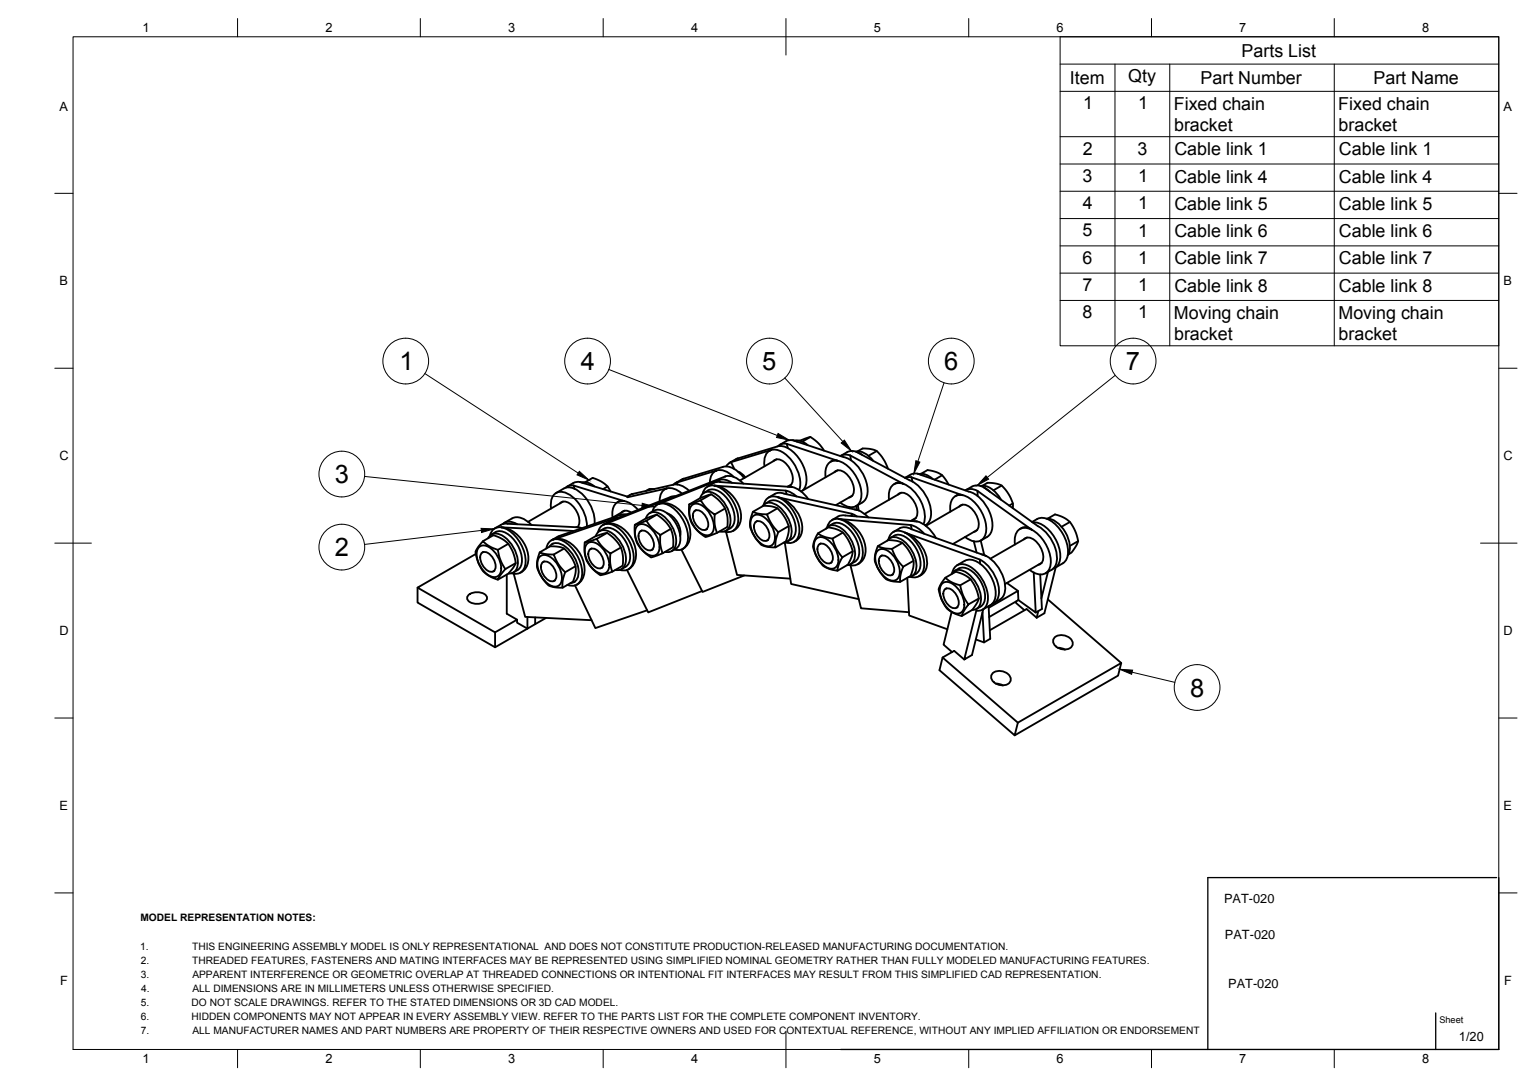
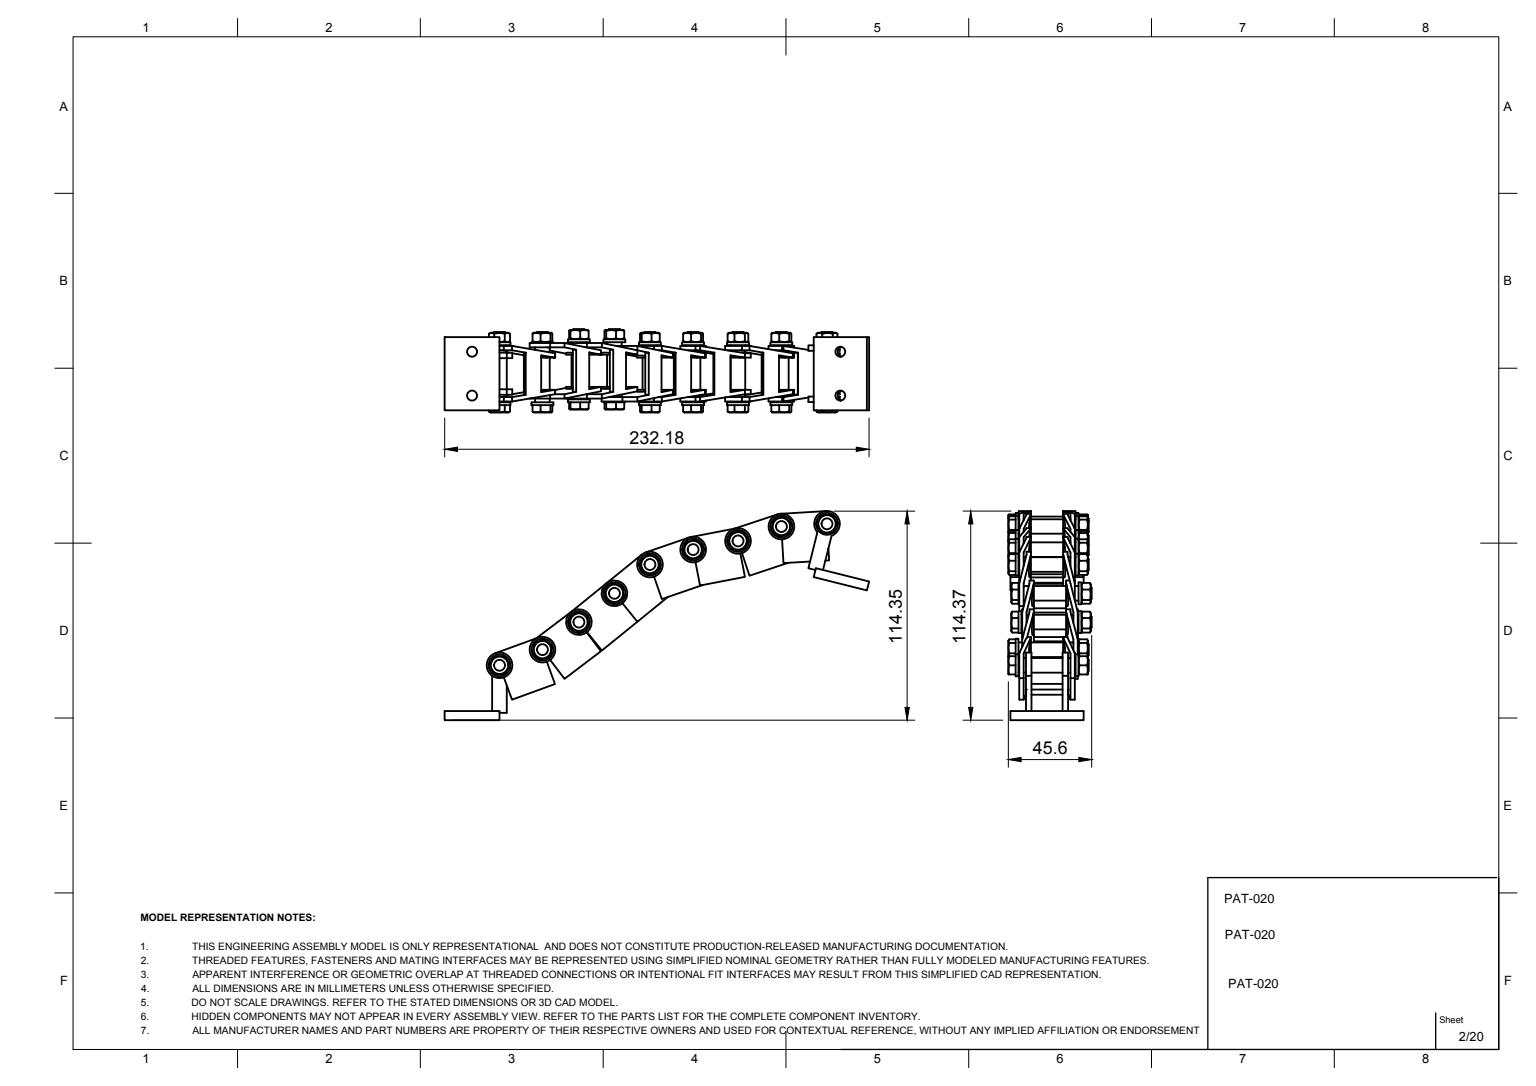
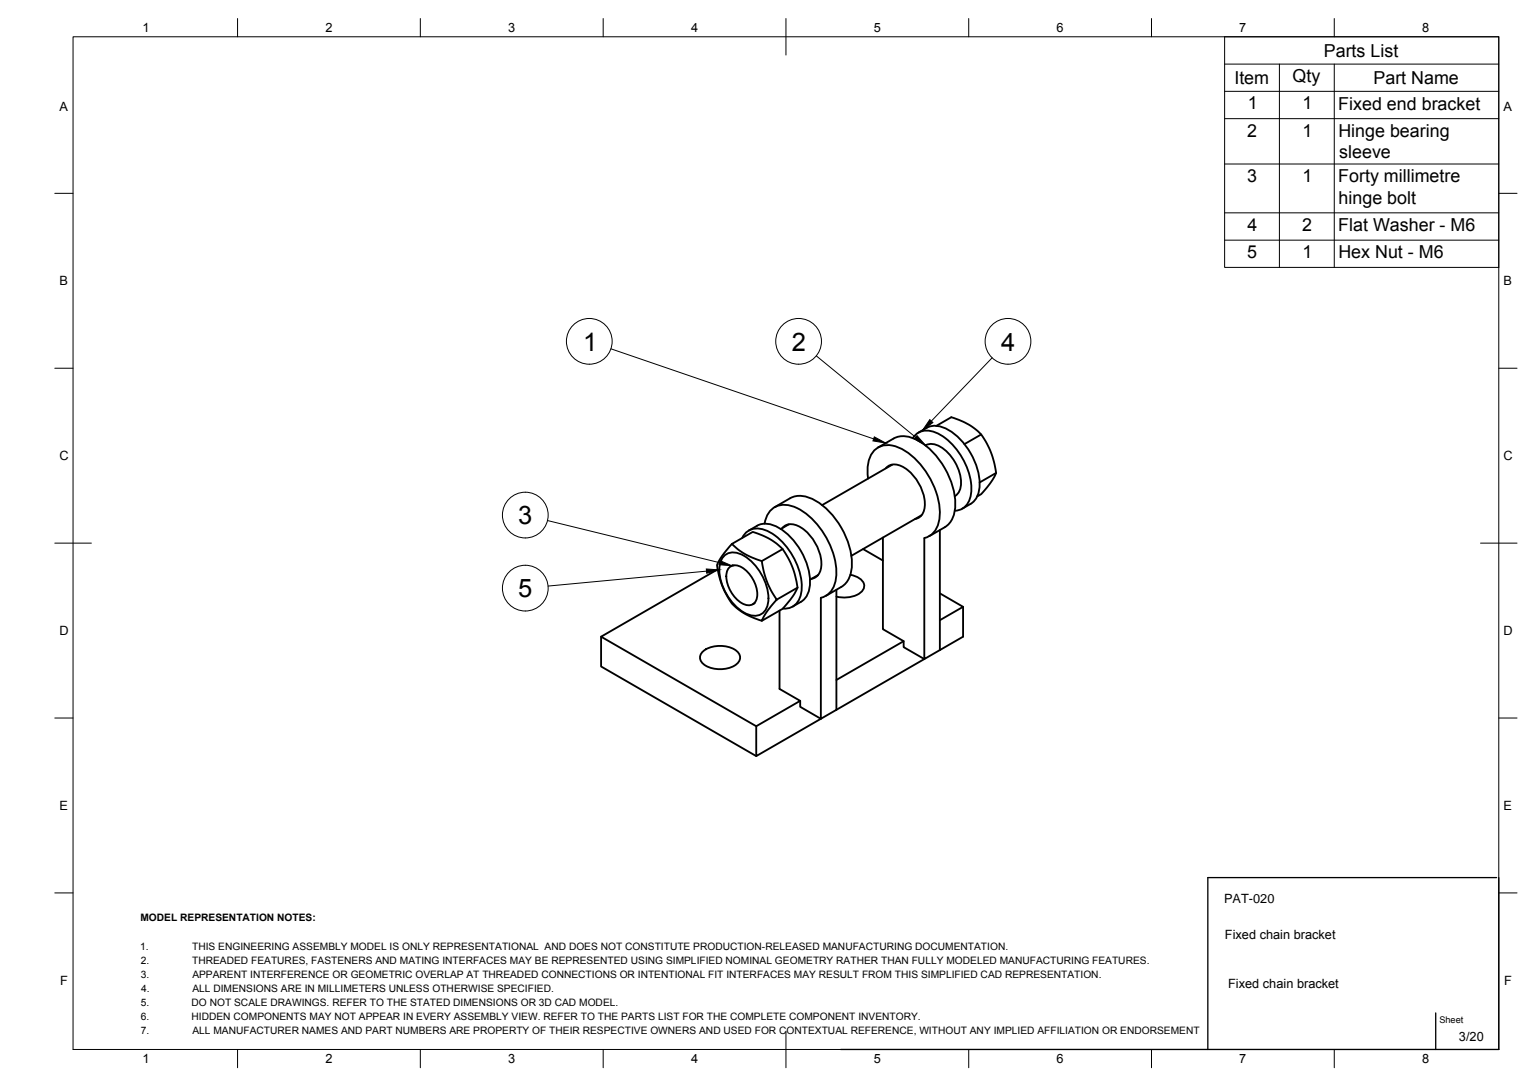
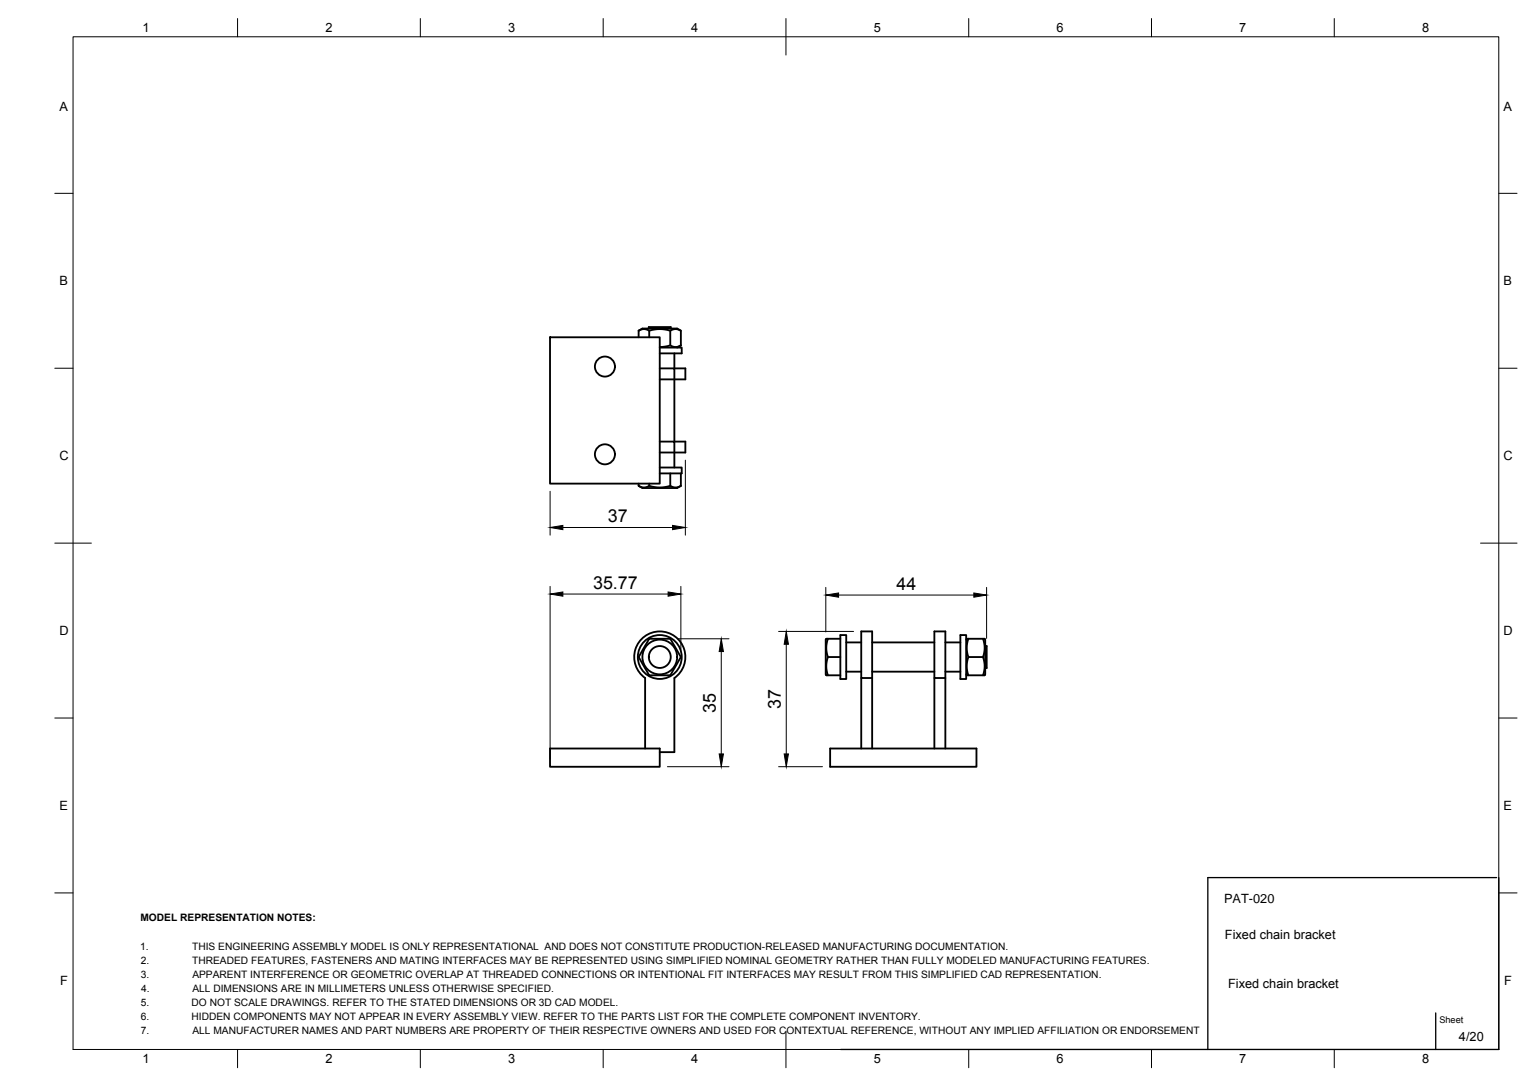
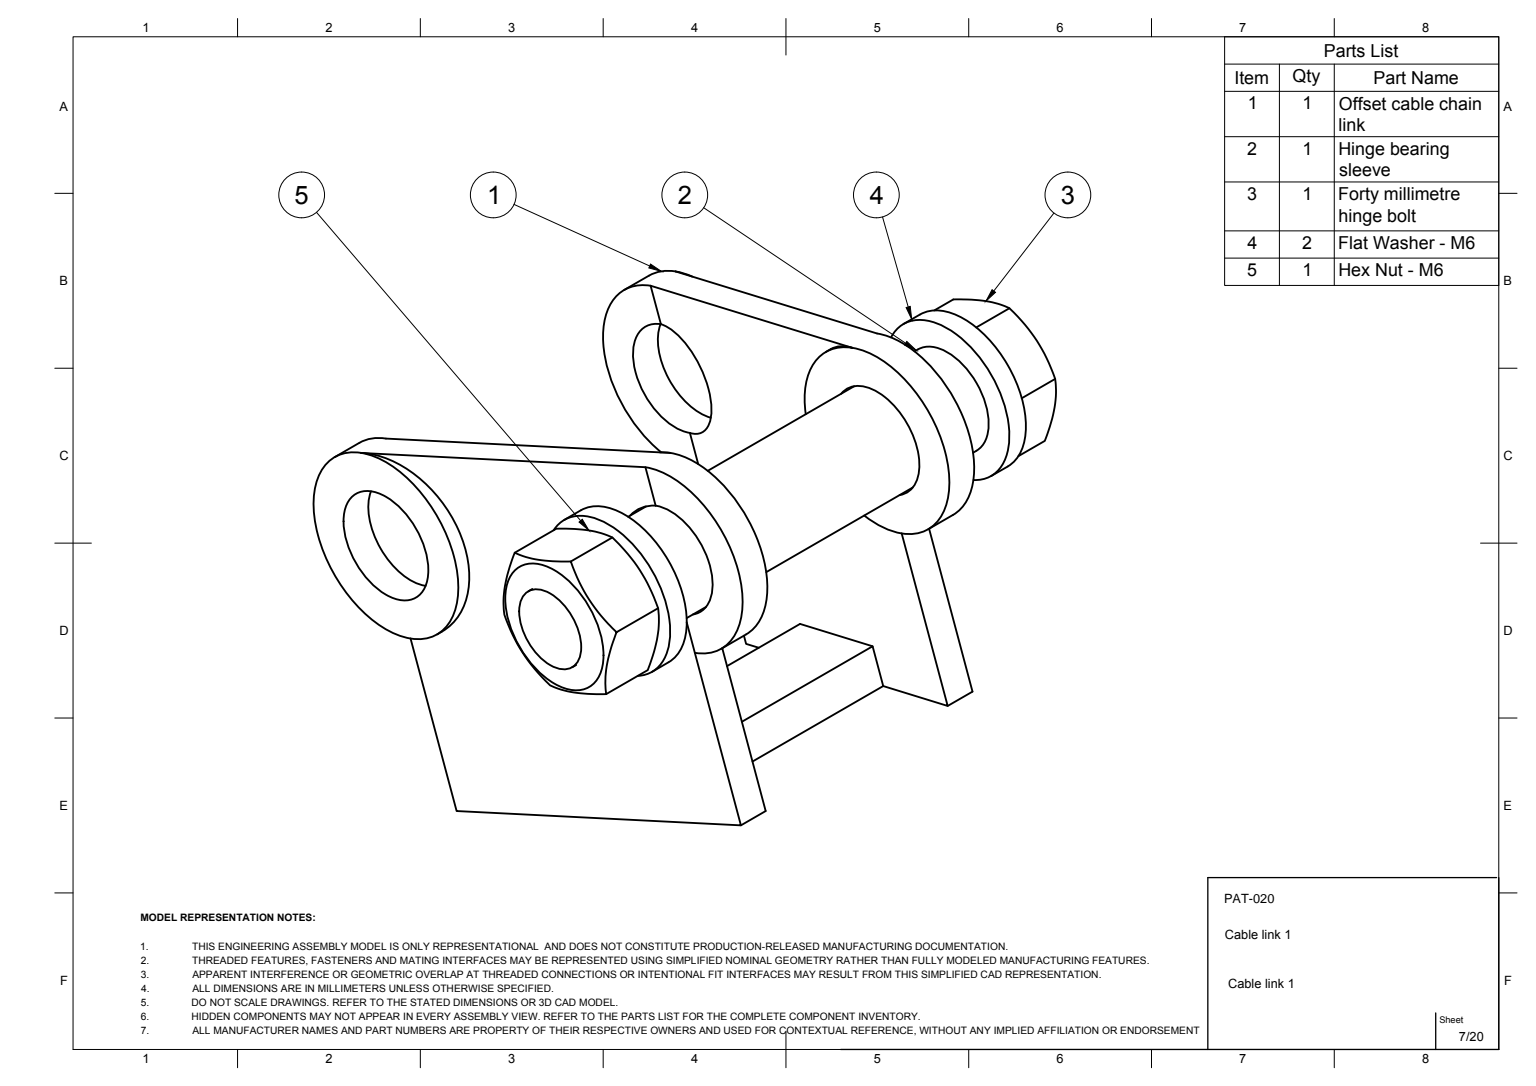
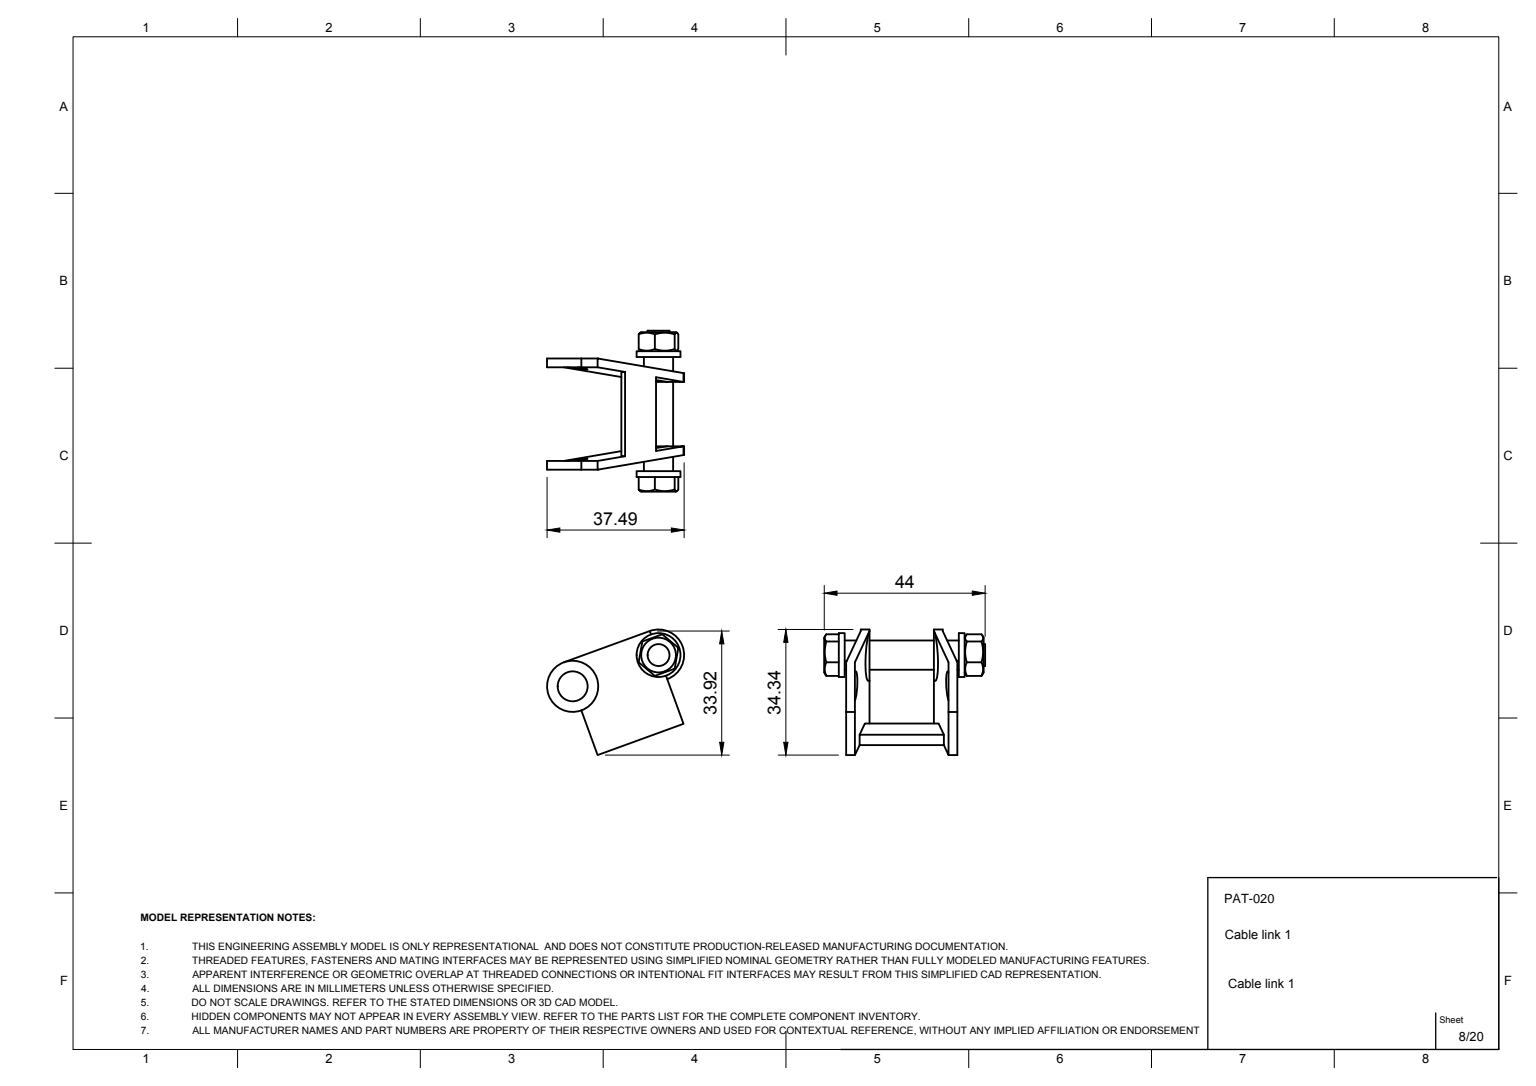
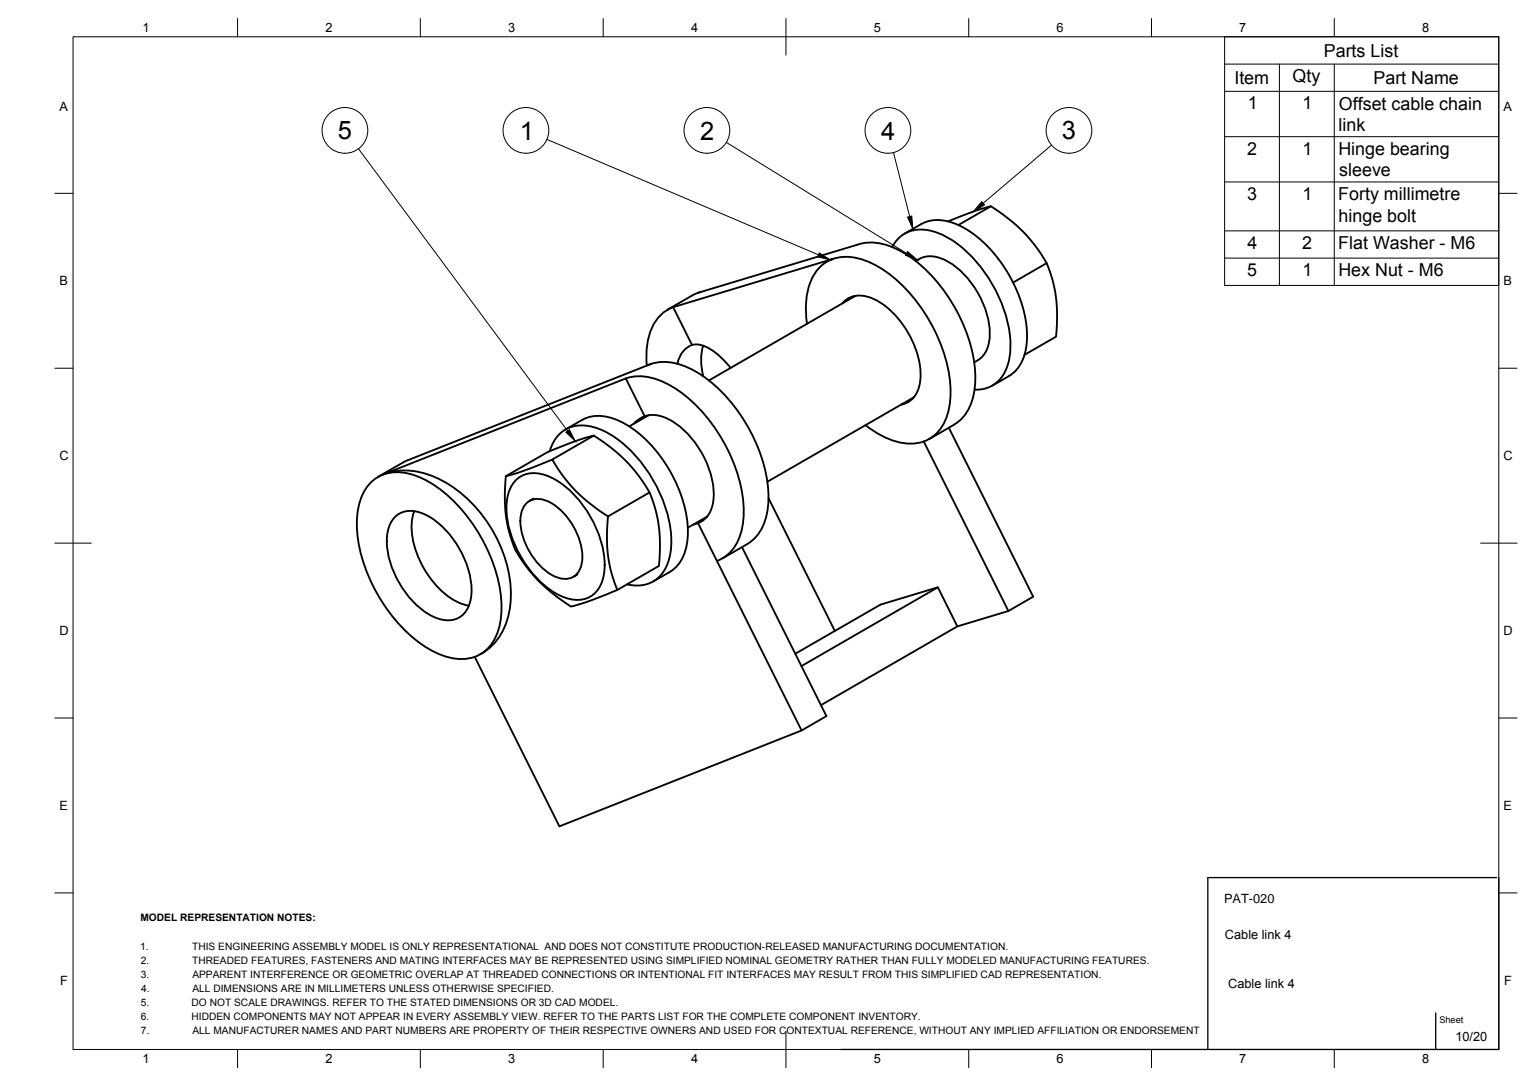
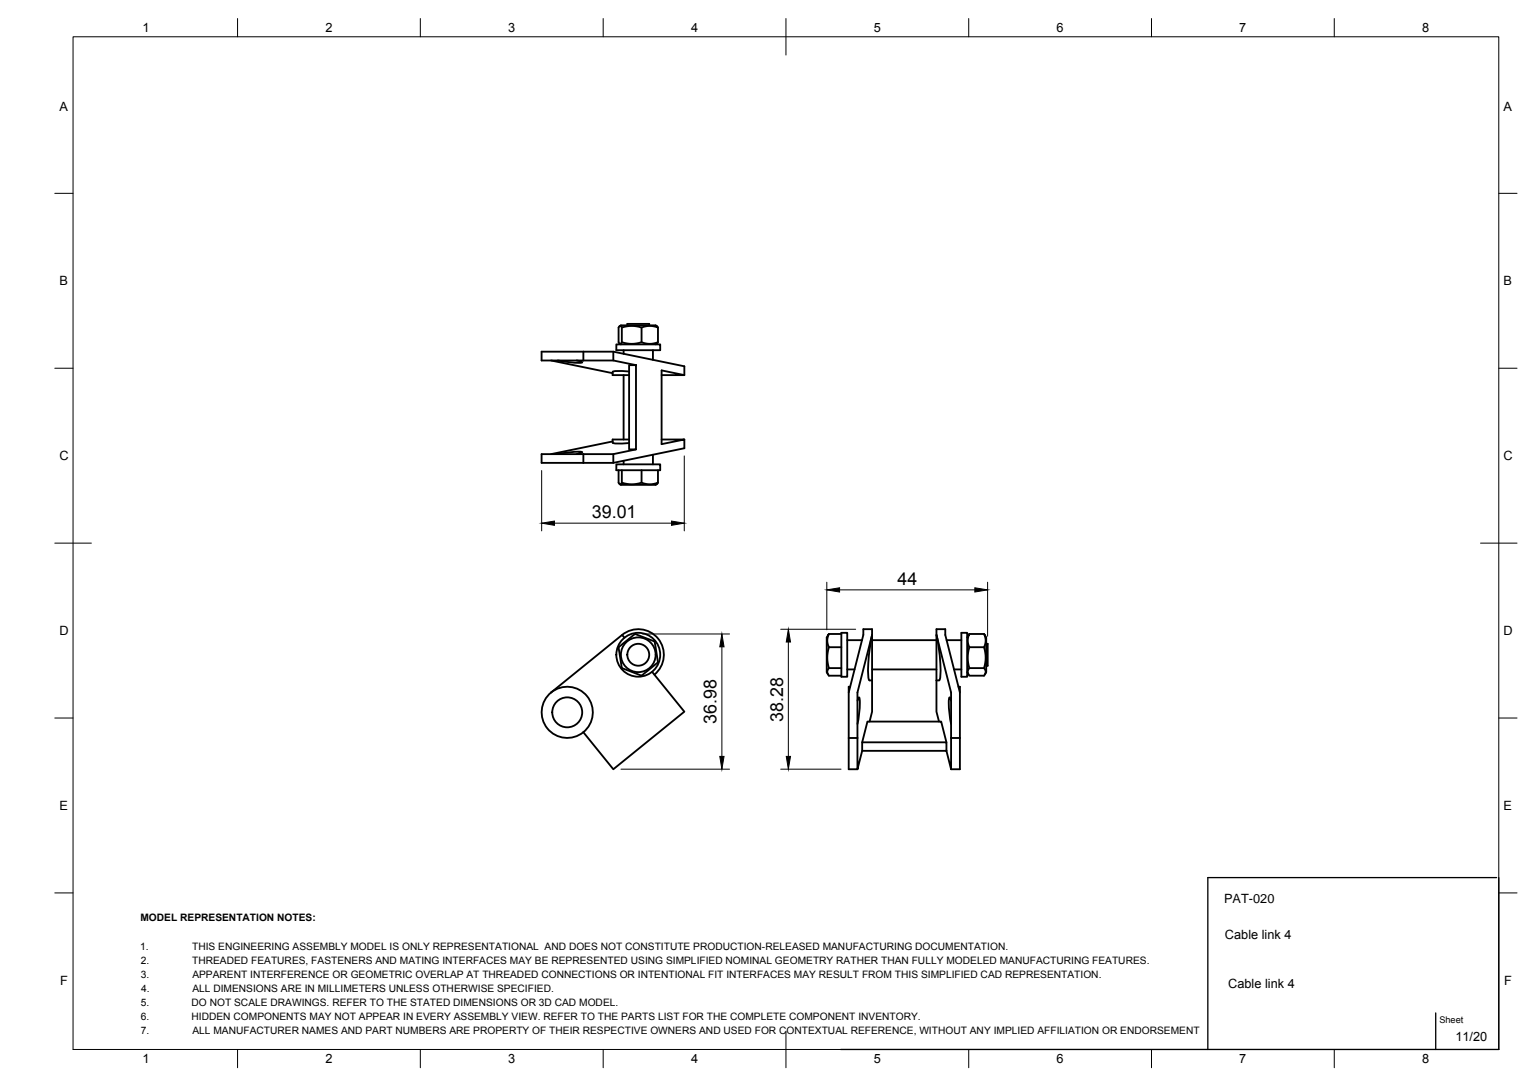
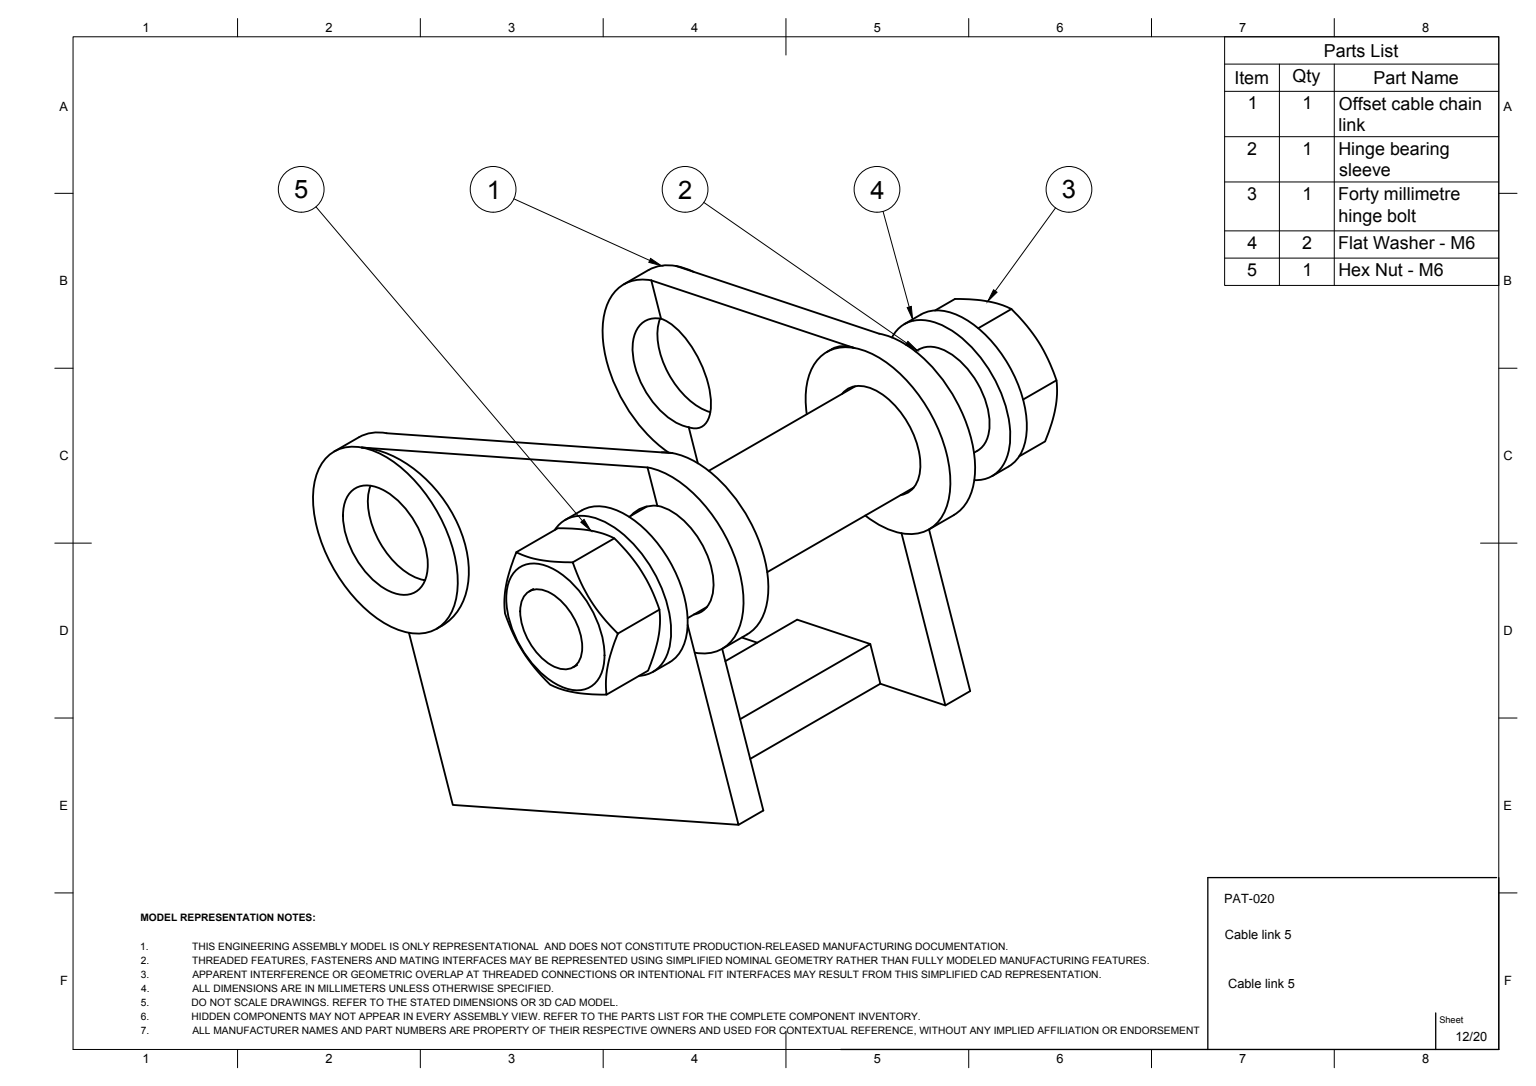
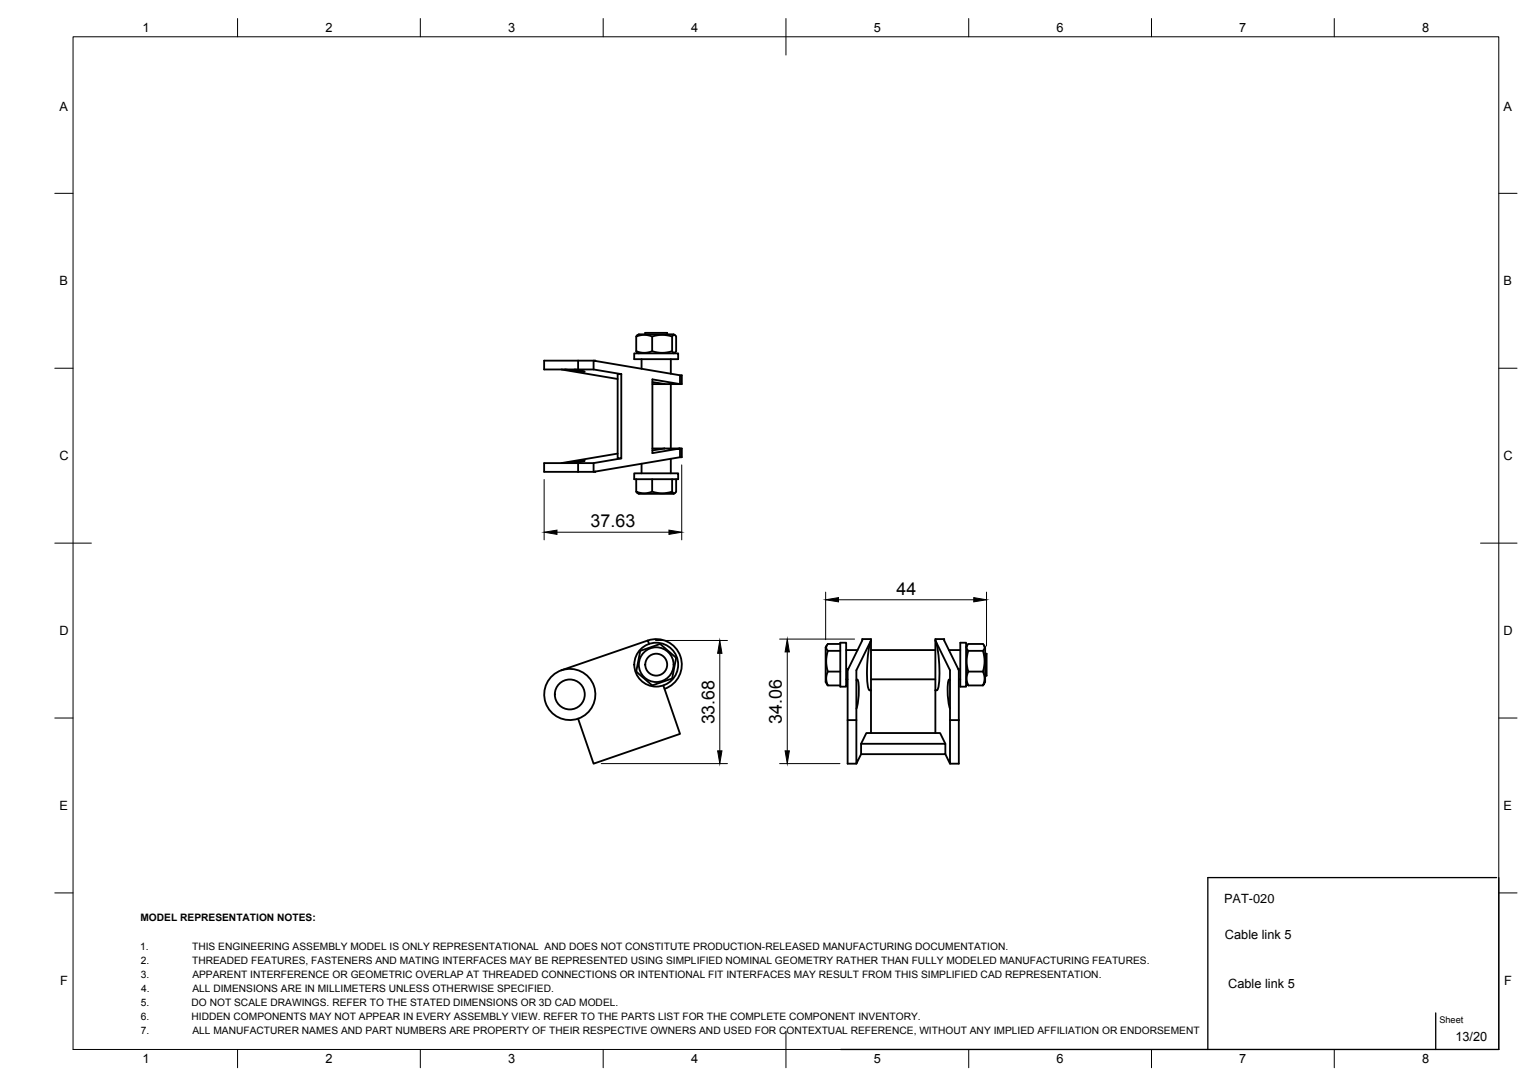
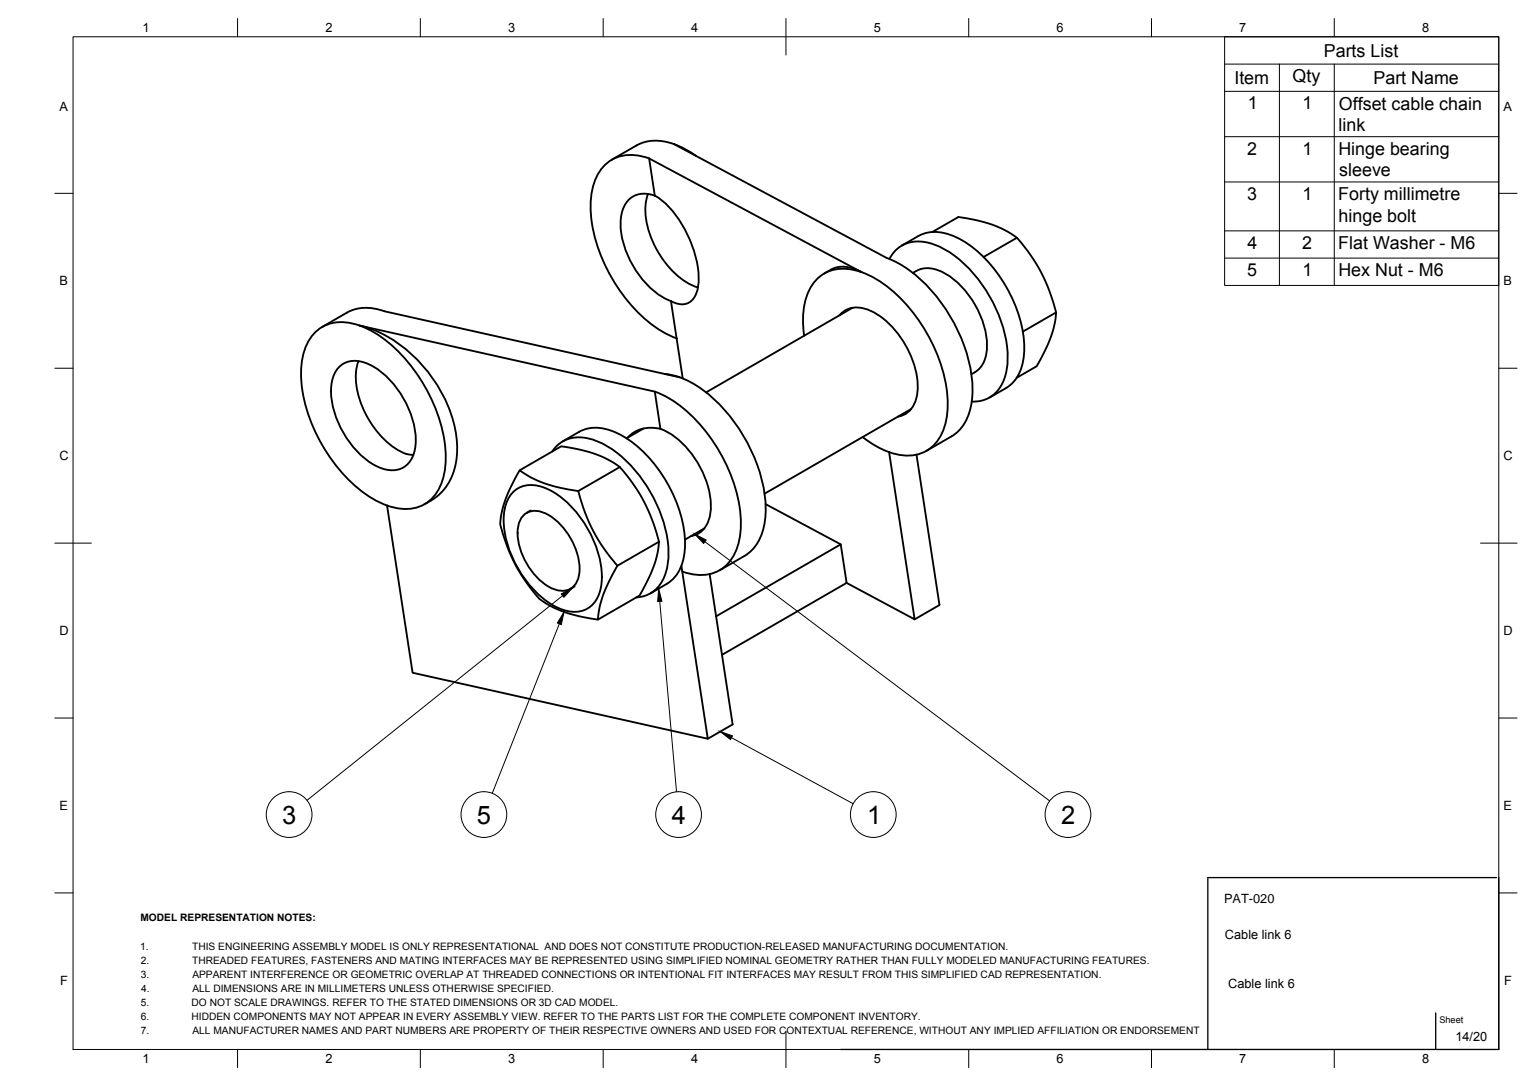
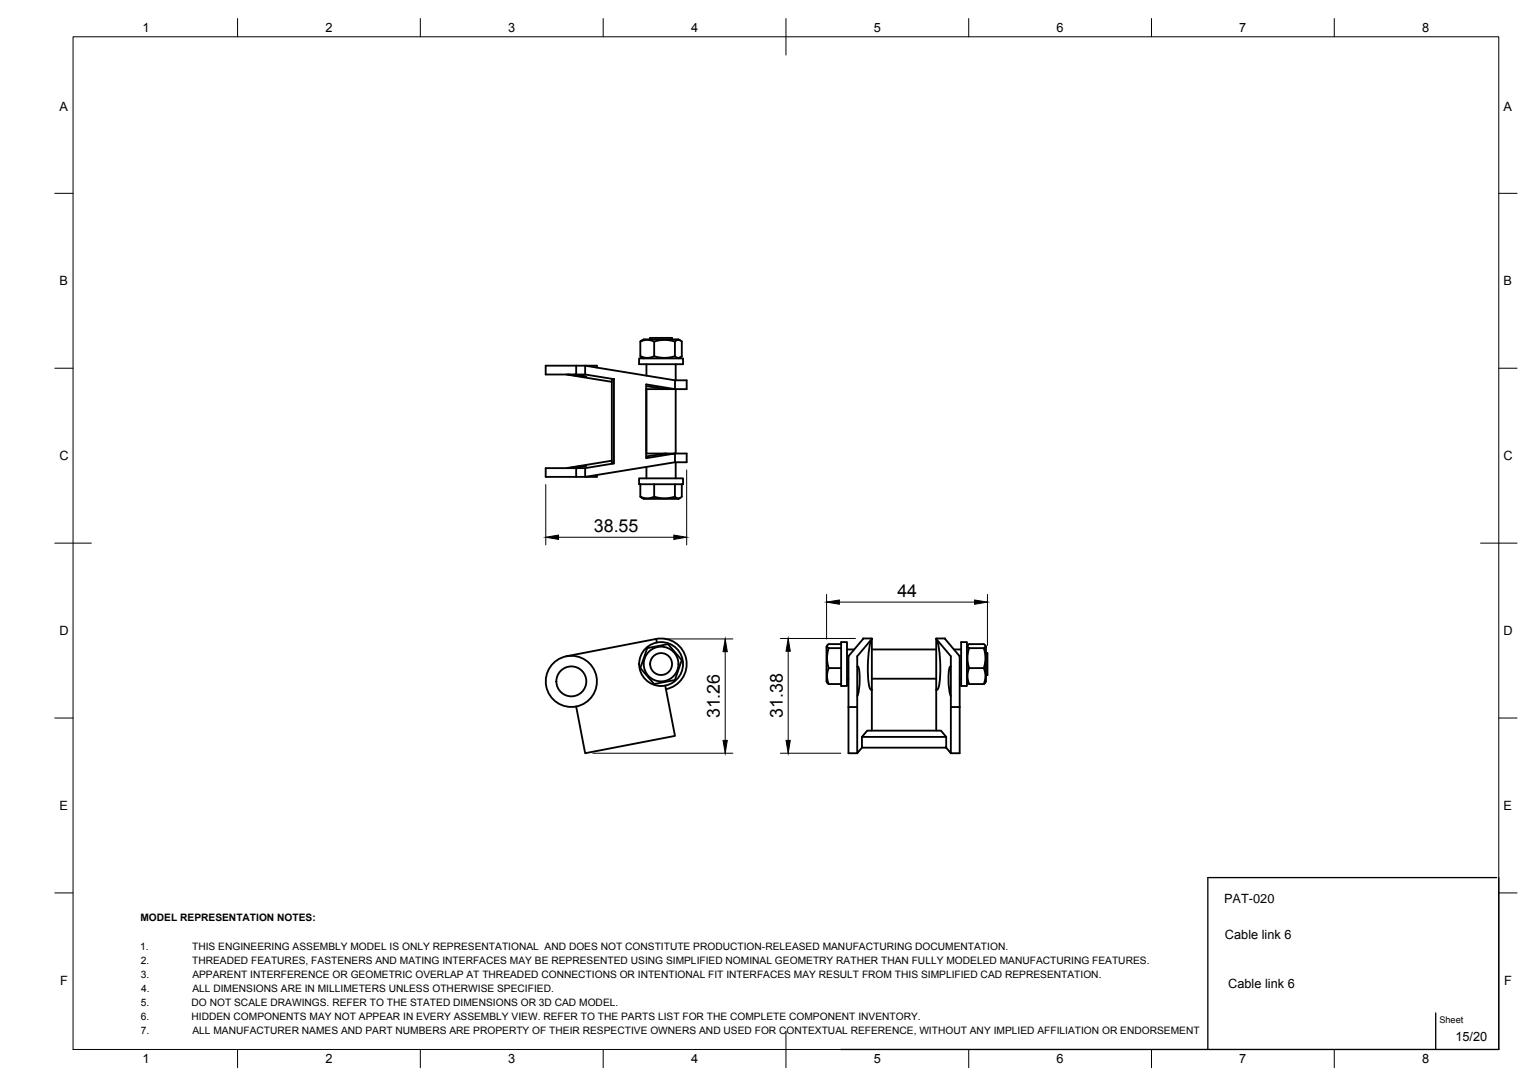
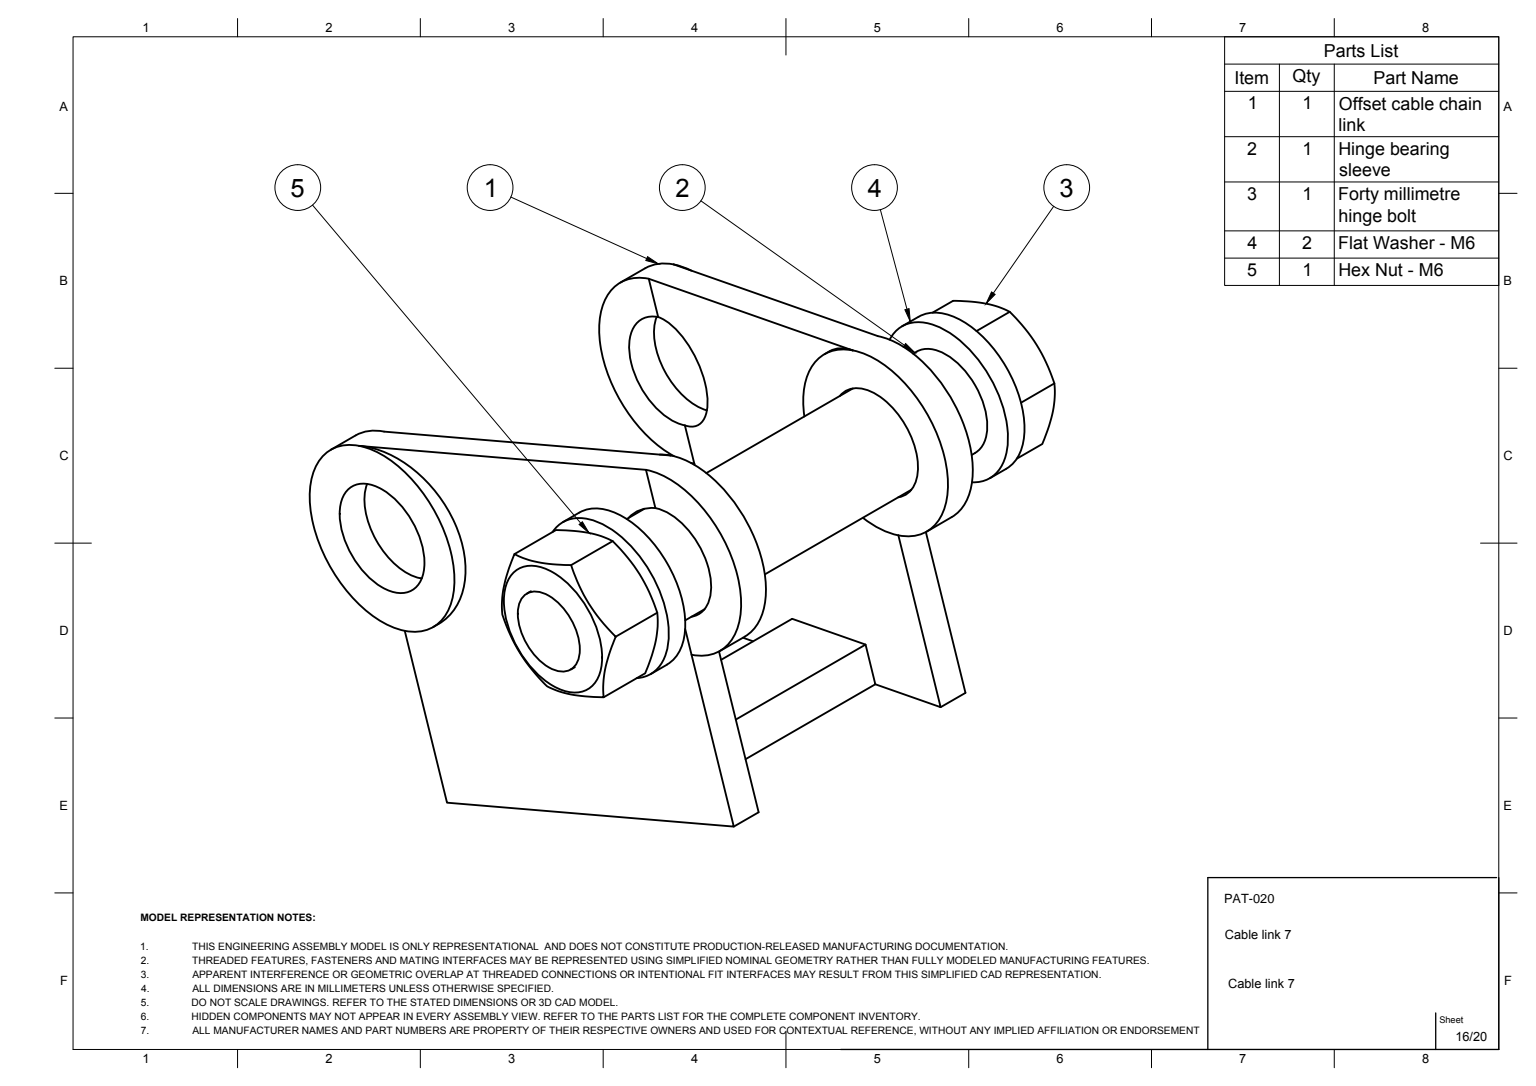
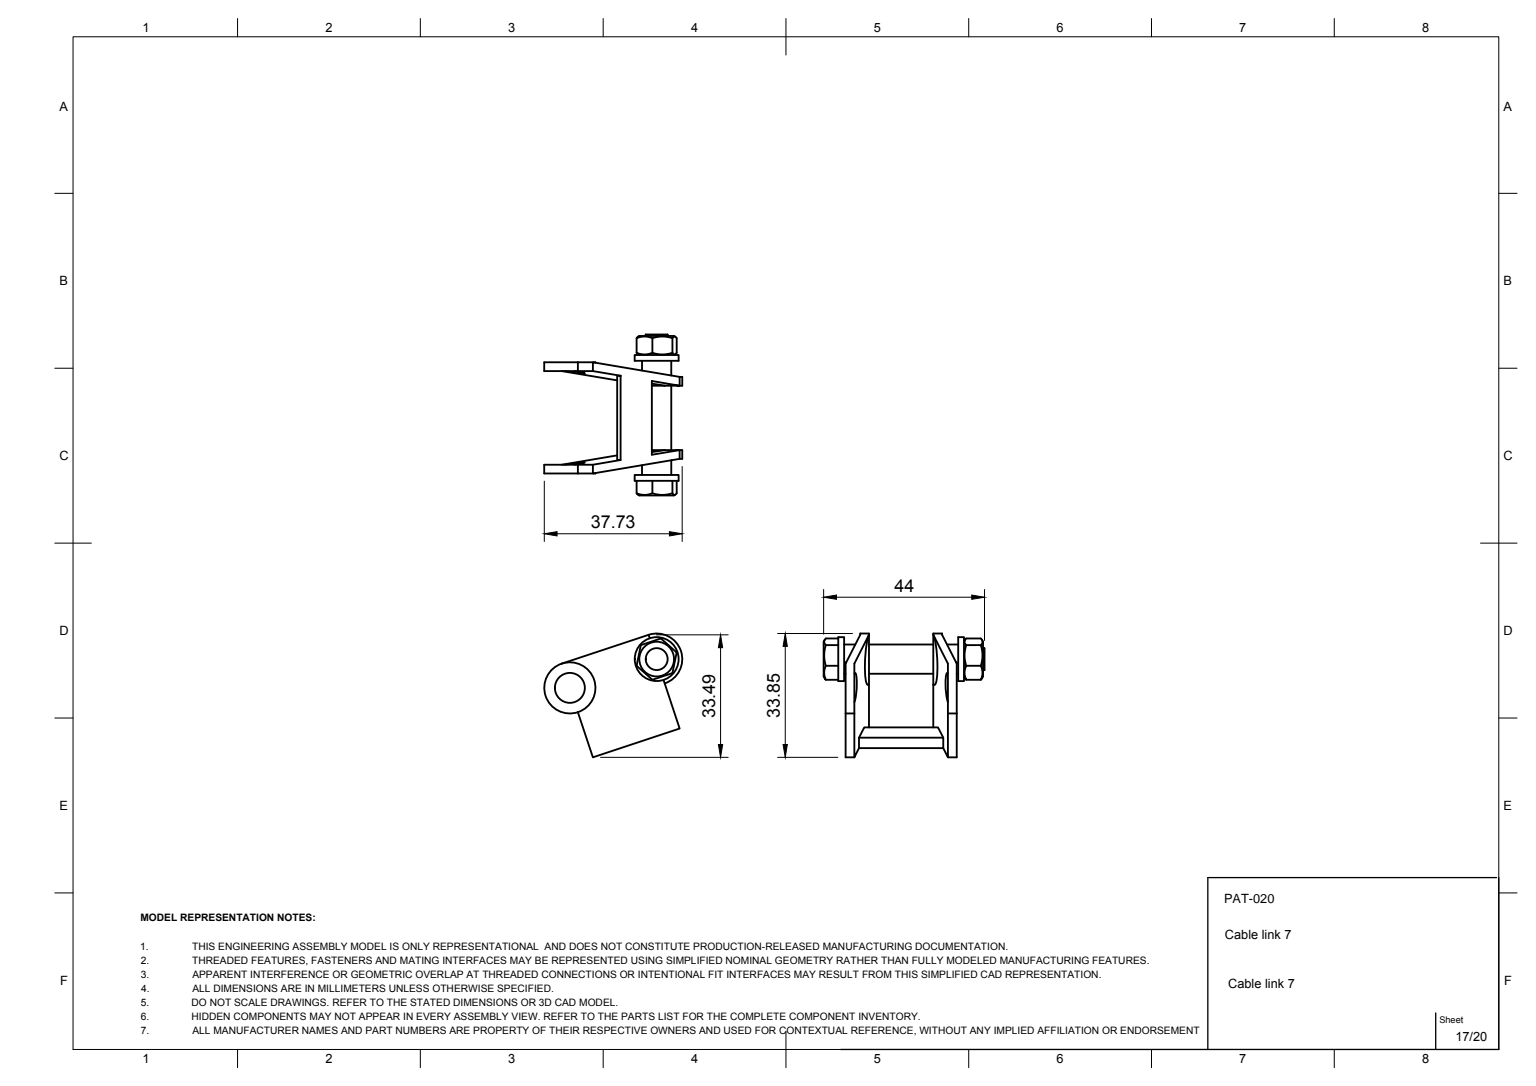
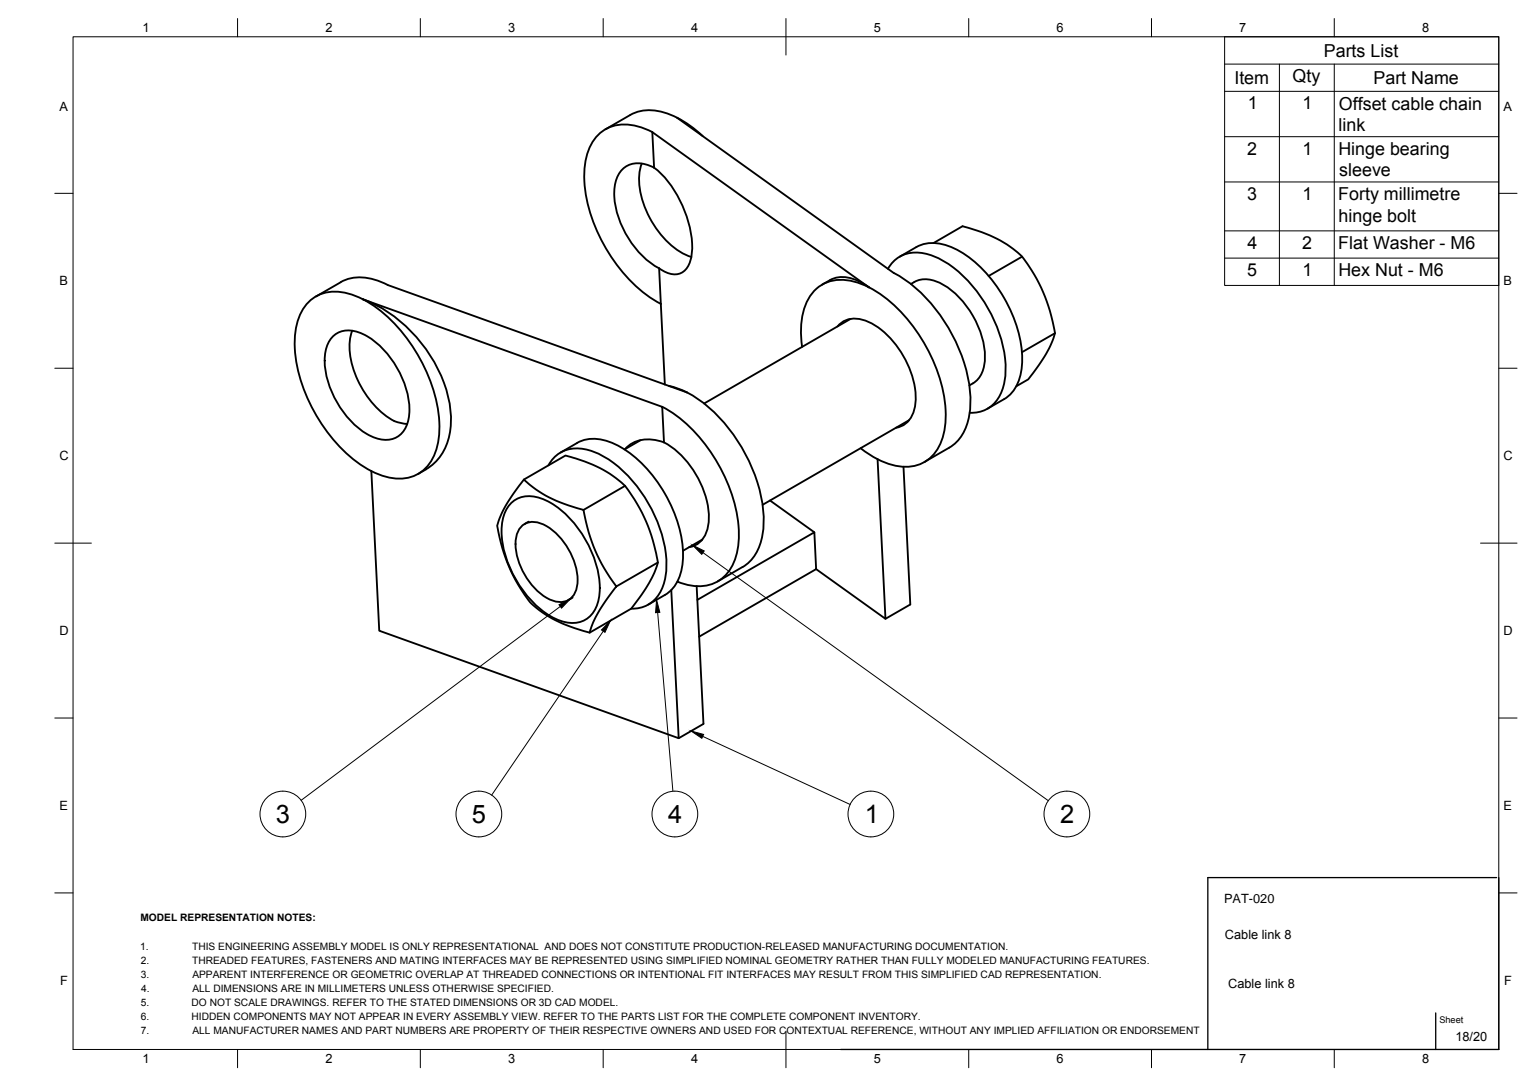
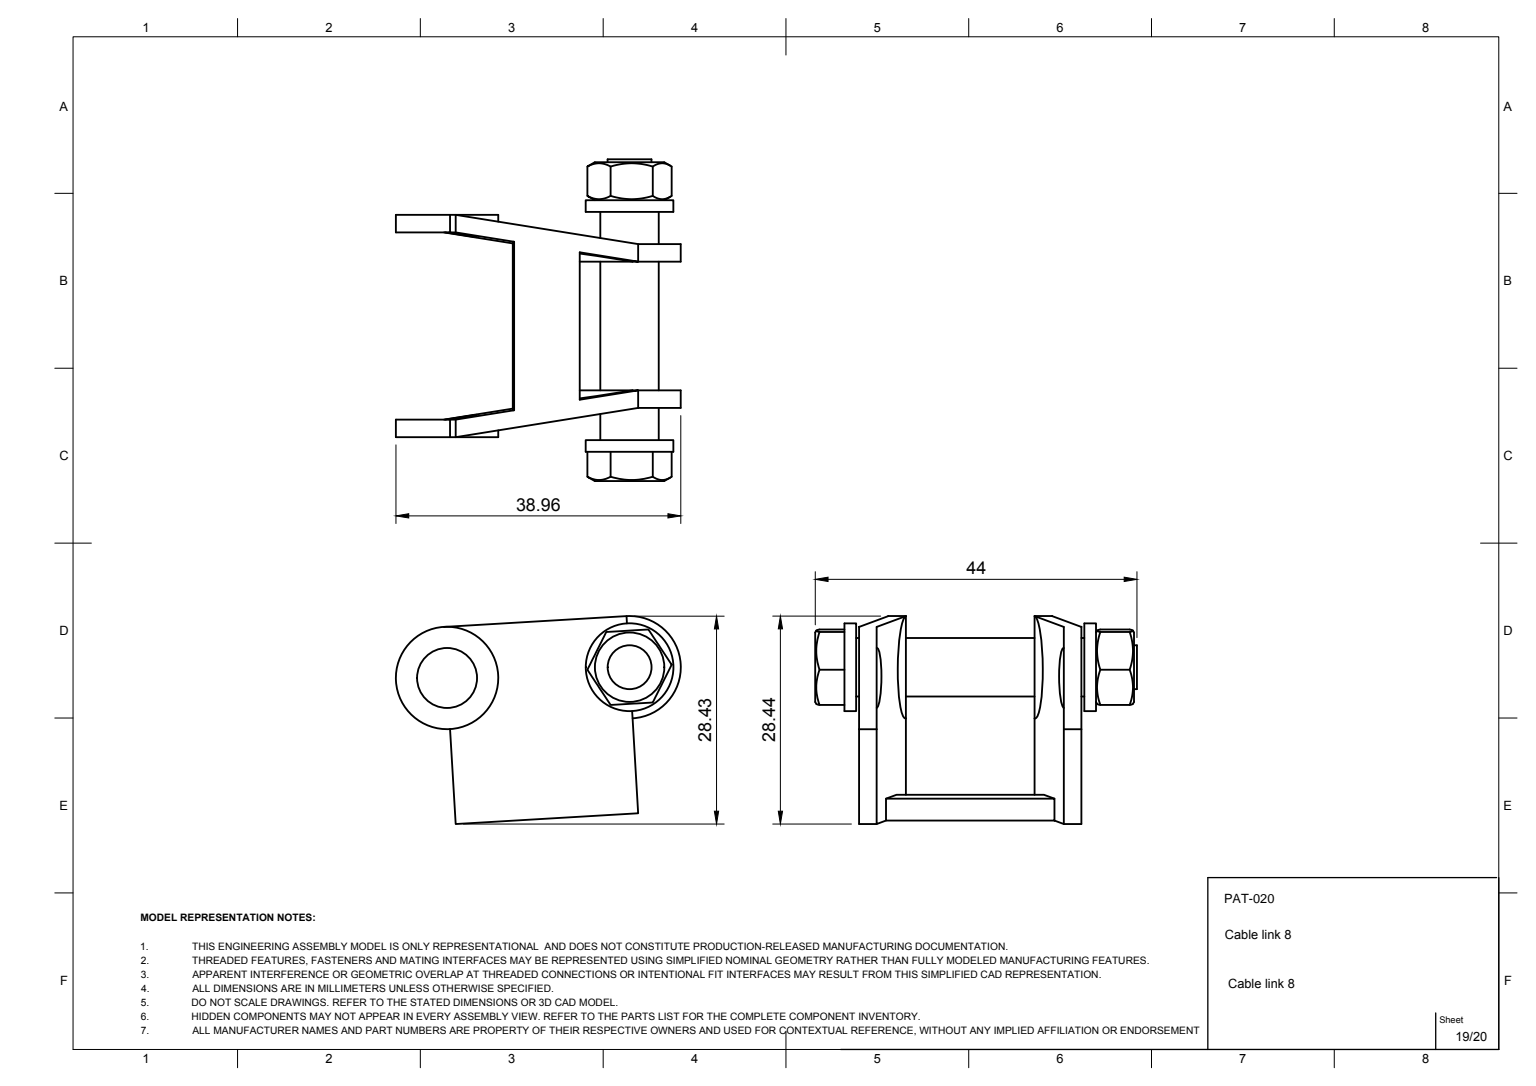
ISO-10303-21;
HEADER;
/* Generated by software containing ST-Developer
 * from STEP Tools, Inc. (www.steptools.com) 
 */

FILE_DESCRIPTION(
/* description */ ('Cable chain and bracket set'),
/* implementation_level */ '2;1');

FILE_NAME(
/* name */ 'PAT-020',
/* time_stamp */ '2026-10-29T17:19:47-07:00',
/* author */ (''),
/* organization */ (''),
/* preprocessor_version */ 'ST-DEVELOPER v20.2',
/* originating_system */ 'Autodesk Translation Framework v15.17.0.0',
/* authorisation */ '');

FILE_SCHEMA (('AUTOMOTIVE_DESIGN { 1 0 10303 214 3 1 1 }'));
ENDSEC;

DATA;
#10=MECHANICAL_DESIGN_GEOMETRIC_PRESENTATION_REPRESENTATION('',(#337,#338,
#339,#340,#341,#342,#343,#344,#345,#346,#347,#348,#349),#5929);
#11=ITEM_DEFINED_TRANSFORMATION($,$,#3460,#3591);
#12=ITEM_DEFINED_TRANSFORMATION($,$,#3527,#3592);
#13=ITEM_DEFINED_TRANSFORMATION($,$,#3536,#3593);
#14=ITEM_DEFINED_TRANSFORMATION($,$,#3557,#3594);
#15=ITEM_DEFINED_TRANSFORMATION($,$,#3566,#3595);
#16=ITEM_DEFINED_TRANSFORMATION($,$,#3575,#3596);
#17=ITEM_DEFINED_TRANSFORMATION($,$,#3603,#3638);
#18=ITEM_DEFINED_TRANSFORMATION($,$,#3424,#3762);
#19=ITEM_DEFINED_TRANSFORMATION($,$,#3707,#3763);
#20=ITEM_DEFINED_TRANSFORMATION($,$,#3716,#3764);
#21=ITEM_DEFINED_TRANSFORMATION($,$,#3737,#3765);
#22=ITEM_DEFINED_TRANSFORMATION($,$,#3737,#3766);
#23=ITEM_DEFINED_TRANSFORMATION($,$,#3746,#3767);
#24=ITEM_DEFINED_TRANSFORMATION($,$,#3640,#3768);
#25=ITEM_DEFINED_TRANSFORMATION($,$,#3707,#3769);
#26=ITEM_DEFINED_TRANSFORMATION($,$,#3716,#3770);
#27=ITEM_DEFINED_TRANSFORMATION($,$,#3737,#3771);
#28=ITEM_DEFINED_TRANSFORMATION($,$,#3737,#3772);
#29=ITEM_DEFINED_TRANSFORMATION($,$,#3746,#3773);
#30=ITEM_DEFINED_TRANSFORMATION($,$,#3640,#3774);
#31=ITEM_DEFINED_TRANSFORMATION($,$,#3707,#3775);
#32=ITEM_DEFINED_TRANSFORMATION($,$,#3716,#3776);
#33=ITEM_DEFINED_TRANSFORMATION($,$,#3737,#3777);
#34=ITEM_DEFINED_TRANSFORMATION($,$,#3737,#3778);
#35=ITEM_DEFINED_TRANSFORMATION($,$,#3746,#3779);
#36=ITEM_DEFINED_TRANSFORMATION($,$,#3640,#3780);
#37=ITEM_DEFINED_TRANSFORMATION($,$,#3707,#3781);
#38=ITEM_DEFINED_TRANSFORMATION($,$,#3716,#3782);
#39=ITEM_DEFINED_TRANSFORMATION($,$,#3737,#3783);
#40=ITEM_DEFINED_TRANSFORMATION($,$,#3737,#3784);
#41=ITEM_DEFINED_TRANSFORMATION($,$,#3746,#3785);
#42=ITEM_DEFINED_TRANSFORMATION($,$,#3640,#3786);
#43=ITEM_DEFINED_TRANSFORMATION($,$,#3707,#3787);
#44=ITEM_DEFINED_TRANSFORMATION($,$,#3716,#3788);
#45=ITEM_DEFINED_TRANSFORMATION($,$,#3737,#3789);
#46=ITEM_DEFINED_TRANSFORMATION($,$,#3737,#3790);
#47=ITEM_DEFINED_TRANSFORMATION($,$,#3746,#3791);
#48=ITEM_DEFINED_TRANSFORMATION($,$,#3640,#3792);
#49=ITEM_DEFINED_TRANSFORMATION($,$,#3707,#3793);
#50=ITEM_DEFINED_TRANSFORMATION($,$,#3716,#3794);
#51=ITEM_DEFINED_TRANSFORMATION($,$,#3737,#3795);
#52=ITEM_DEFINED_TRANSFORMATION($,$,#3737,#3796);
#53=ITEM_DEFINED_TRANSFORMATION($,$,#3746,#3797);
#54=ITEM_DEFINED_TRANSFORMATION($,$,#3640,#3798);
#55=ITEM_DEFINED_TRANSFORMATION($,$,#3707,#3799);
#56=ITEM_DEFINED_TRANSFORMATION($,$,#3716,#3800);
#57=ITEM_DEFINED_TRANSFORMATION($,$,#3737,#3801);
#58=ITEM_DEFINED_TRANSFORMATION($,$,#3737,#3802);
#59=ITEM_DEFINED_TRANSFORMATION($,$,#3746,#3803);
#60=ITEM_DEFINED_TRANSFORMATION($,$,#3423,#3804);
#61=ITEM_DEFINED_TRANSFORMATION($,$,#3459,#3805);
#62=ITEM_DEFINED_TRANSFORMATION($,$,#3597,#3806);
#63=ITEM_DEFINED_TRANSFORMATION($,$,#3598,#3807);
#64=ITEM_DEFINED_TRANSFORMATION($,$,#3599,#3808);
#65=ITEM_DEFINED_TRANSFORMATION($,$,#3600,#3809);
#66=ITEM_DEFINED_TRANSFORMATION($,$,#3601,#3810);
#67=ITEM_DEFINED_TRANSFORMATION($,$,#3602,#3811);
#68=ITEM_DEFINED_TRANSFORMATION($,$,#3639,#3812);
#69=ITEM_DEFINED_TRANSFORMATION($,$,#3639,#3813);
#70=(
REPRESENTATION_RELATIONSHIP($,$,#6043,#6042)
REPRESENTATION_RELATIONSHIP_WITH_TRANSFORMATION(#11)
SHAPE_REPRESENTATION_RELATIONSHIP()
);
#71=(
REPRESENTATION_RELATIONSHIP($,$,#6044,#6042)
REPRESENTATION_RELATIONSHIP_WITH_TRANSFORMATION(#12)
SHAPE_REPRESENTATION_RELATIONSHIP()
);
#72=(
REPRESENTATION_RELATIONSHIP($,$,#6045,#6042)
REPRESENTATION_RELATIONSHIP_WITH_TRANSFORMATION(#13)
SHAPE_REPRESENTATION_RELATIONSHIP()
);
#73=(
REPRESENTATION_RELATIONSHIP($,$,#6046,#6042)
REPRESENTATION_RELATIONSHIP_WITH_TRANSFORMATION(#14)
SHAPE_REPRESENTATION_RELATIONSHIP()
);
#74=(
REPRESENTATION_RELATIONSHIP($,$,#6047,#6042)
REPRESENTATION_RELATIONSHIP_WITH_TRANSFORMATION(#15)
SHAPE_REPRESENTATION_RELATIONSHIP()
);
#75=(
REPRESENTATION_RELATIONSHIP($,$,#6048,#6042)
REPRESENTATION_RELATIONSHIP_WITH_TRANSFORMATION(#16)
SHAPE_REPRESENTATION_RELATIONSHIP()
);
#76=(
REPRESENTATION_RELATIONSHIP($,$,#6055,#6054)
REPRESENTATION_RELATIONSHIP_WITH_TRANSFORMATION(#17)
SHAPE_REPRESENTATION_RELATIONSHIP()
);
#77=(
REPRESENTATION_RELATIONSHIP($,$,#6041,#6040)
REPRESENTATION_RELATIONSHIP_WITH_TRANSFORMATION(#18)
SHAPE_REPRESENTATION_RELATIONSHIP()
);
#78=(
REPRESENTATION_RELATIONSHIP($,$,#6058,#6040)
REPRESENTATION_RELATIONSHIP_WITH_TRANSFORMATION(#19)
SHAPE_REPRESENTATION_RELATIONSHIP()
);
#79=(
REPRESENTATION_RELATIONSHIP($,$,#6059,#6040)
REPRESENTATION_RELATIONSHIP_WITH_TRANSFORMATION(#20)
SHAPE_REPRESENTATION_RELATIONSHIP()
);
#80=(
REPRESENTATION_RELATIONSHIP($,$,#6060,#6040)
REPRESENTATION_RELATIONSHIP_WITH_TRANSFORMATION(#21)
SHAPE_REPRESENTATION_RELATIONSHIP()
);
#81=(
REPRESENTATION_RELATIONSHIP($,$,#6060,#6040)
REPRESENTATION_RELATIONSHIP_WITH_TRANSFORMATION(#22)
SHAPE_REPRESENTATION_RELATIONSHIP()
);
#82=(
REPRESENTATION_RELATIONSHIP($,$,#6061,#6040)
REPRESENTATION_RELATIONSHIP_WITH_TRANSFORMATION(#23)
SHAPE_REPRESENTATION_RELATIONSHIP()
);
#83=(
REPRESENTATION_RELATIONSHIP($,$,#6057,#6049)
REPRESENTATION_RELATIONSHIP_WITH_TRANSFORMATION(#24)
SHAPE_REPRESENTATION_RELATIONSHIP()
);
#84=(
REPRESENTATION_RELATIONSHIP($,$,#6058,#6049)
REPRESENTATION_RELATIONSHIP_WITH_TRANSFORMATION(#25)
SHAPE_REPRESENTATION_RELATIONSHIP()
);
#85=(
REPRESENTATION_RELATIONSHIP($,$,#6059,#6049)
REPRESENTATION_RELATIONSHIP_WITH_TRANSFORMATION(#26)
SHAPE_REPRESENTATION_RELATIONSHIP()
);
#86=(
REPRESENTATION_RELATIONSHIP($,$,#6060,#6049)
REPRESENTATION_RELATIONSHIP_WITH_TRANSFORMATION(#27)
SHAPE_REPRESENTATION_RELATIONSHIP()
);
#87=(
REPRESENTATION_RELATIONSHIP($,$,#6060,#6049)
REPRESENTATION_RELATIONSHIP_WITH_TRANSFORMATION(#28)
SHAPE_REPRESENTATION_RELATIONSHIP()
);
#88=(
REPRESENTATION_RELATIONSHIP($,$,#6061,#6049)
REPRESENTATION_RELATIONSHIP_WITH_TRANSFORMATION(#29)
SHAPE_REPRESENTATION_RELATIONSHIP()
);
#89=(
REPRESENTATION_RELATIONSHIP($,$,#6057,#6050)
REPRESENTATION_RELATIONSHIP_WITH_TRANSFORMATION(#30)
SHAPE_REPRESENTATION_RELATIONSHIP()
);
#90=(
REPRESENTATION_RELATIONSHIP($,$,#6058,#6050)
REPRESENTATION_RELATIONSHIP_WITH_TRANSFORMATION(#31)
SHAPE_REPRESENTATION_RELATIONSHIP()
);
#91=(
REPRESENTATION_RELATIONSHIP($,$,#6059,#6050)
REPRESENTATION_RELATIONSHIP_WITH_TRANSFORMATION(#32)
SHAPE_REPRESENTATION_RELATIONSHIP()
);
#92=(
REPRESENTATION_RELATIONSHIP($,$,#6060,#6050)
REPRESENTATION_RELATIONSHIP_WITH_TRANSFORMATION(#33)
SHAPE_REPRESENTATION_RELATIONSHIP()
);
#93=(
REPRESENTATION_RELATIONSHIP($,$,#6060,#6050)
REPRESENTATION_RELATIONSHIP_WITH_TRANSFORMATION(#34)
SHAPE_REPRESENTATION_RELATIONSHIP()
);
#94=(
REPRESENTATION_RELATIONSHIP($,$,#6061,#6050)
REPRESENTATION_RELATIONSHIP_WITH_TRANSFORMATION(#35)
SHAPE_REPRESENTATION_RELATIONSHIP()
);
#95=(
REPRESENTATION_RELATIONSHIP($,$,#6057,#6051)
REPRESENTATION_RELATIONSHIP_WITH_TRANSFORMATION(#36)
SHAPE_REPRESENTATION_RELATIONSHIP()
);
#96=(
REPRESENTATION_RELATIONSHIP($,$,#6058,#6051)
REPRESENTATION_RELATIONSHIP_WITH_TRANSFORMATION(#37)
SHAPE_REPRESENTATION_RELATIONSHIP()
);
#97=(
REPRESENTATION_RELATIONSHIP($,$,#6059,#6051)
REPRESENTATION_RELATIONSHIP_WITH_TRANSFORMATION(#38)
SHAPE_REPRESENTATION_RELATIONSHIP()
);
#98=(
REPRESENTATION_RELATIONSHIP($,$,#6060,#6051)
REPRESENTATION_RELATIONSHIP_WITH_TRANSFORMATION(#39)
SHAPE_REPRESENTATION_RELATIONSHIP()
);
#99=(
REPRESENTATION_RELATIONSHIP($,$,#6060,#6051)
REPRESENTATION_RELATIONSHIP_WITH_TRANSFORMATION(#40)
SHAPE_REPRESENTATION_RELATIONSHIP()
);
#100=(
REPRESENTATION_RELATIONSHIP($,$,#6061,#6051)
REPRESENTATION_RELATIONSHIP_WITH_TRANSFORMATION(#41)
SHAPE_REPRESENTATION_RELATIONSHIP()
);
#101=(
REPRESENTATION_RELATIONSHIP($,$,#6057,#6052)
REPRESENTATION_RELATIONSHIP_WITH_TRANSFORMATION(#42)
SHAPE_REPRESENTATION_RELATIONSHIP()
);
#102=(
REPRESENTATION_RELATIONSHIP($,$,#6058,#6052)
REPRESENTATION_RELATIONSHIP_WITH_TRANSFORMATION(#43)
SHAPE_REPRESENTATION_RELATIONSHIP()
);
#103=(
REPRESENTATION_RELATIONSHIP($,$,#6059,#6052)
REPRESENTATION_RELATIONSHIP_WITH_TRANSFORMATION(#44)
SHAPE_REPRESENTATION_RELATIONSHIP()
);
#104=(
REPRESENTATION_RELATIONSHIP($,$,#6060,#6052)
REPRESENTATION_RELATIONSHIP_WITH_TRANSFORMATION(#45)
SHAPE_REPRESENTATION_RELATIONSHIP()
);
#105=(
REPRESENTATION_RELATIONSHIP($,$,#6060,#6052)
REPRESENTATION_RELATIONSHIP_WITH_TRANSFORMATION(#46)
SHAPE_REPRESENTATION_RELATIONSHIP()
);
#106=(
REPRESENTATION_RELATIONSHIP($,$,#6061,#6052)
REPRESENTATION_RELATIONSHIP_WITH_TRANSFORMATION(#47)
SHAPE_REPRESENTATION_RELATIONSHIP()
);
#107=(
REPRESENTATION_RELATIONSHIP($,$,#6057,#6053)
REPRESENTATION_RELATIONSHIP_WITH_TRANSFORMATION(#48)
SHAPE_REPRESENTATION_RELATIONSHIP()
);
#108=(
REPRESENTATION_RELATIONSHIP($,$,#6058,#6053)
REPRESENTATION_RELATIONSHIP_WITH_TRANSFORMATION(#49)
SHAPE_REPRESENTATION_RELATIONSHIP()
);
#109=(
REPRESENTATION_RELATIONSHIP($,$,#6059,#6053)
REPRESENTATION_RELATIONSHIP_WITH_TRANSFORMATION(#50)
SHAPE_REPRESENTATION_RELATIONSHIP()
);
#110=(
REPRESENTATION_RELATIONSHIP($,$,#6060,#6053)
REPRESENTATION_RELATIONSHIP_WITH_TRANSFORMATION(#51)
SHAPE_REPRESENTATION_RELATIONSHIP()
);
#111=(
REPRESENTATION_RELATIONSHIP($,$,#6060,#6053)
REPRESENTATION_RELATIONSHIP_WITH_TRANSFORMATION(#52)
SHAPE_REPRESENTATION_RELATIONSHIP()
);
#112=(
REPRESENTATION_RELATIONSHIP($,$,#6061,#6053)
REPRESENTATION_RELATIONSHIP_WITH_TRANSFORMATION(#53)
SHAPE_REPRESENTATION_RELATIONSHIP()
);
#113=(
REPRESENTATION_RELATIONSHIP($,$,#6057,#6056)
REPRESENTATION_RELATIONSHIP_WITH_TRANSFORMATION(#54)
SHAPE_REPRESENTATION_RELATIONSHIP()
);
#114=(
REPRESENTATION_RELATIONSHIP($,$,#6058,#6056)
REPRESENTATION_RELATIONSHIP_WITH_TRANSFORMATION(#55)
SHAPE_REPRESENTATION_RELATIONSHIP()
);
#115=(
REPRESENTATION_RELATIONSHIP($,$,#6059,#6056)
REPRESENTATION_RELATIONSHIP_WITH_TRANSFORMATION(#56)
SHAPE_REPRESENTATION_RELATIONSHIP()
);
#116=(
REPRESENTATION_RELATIONSHIP($,$,#6060,#6056)
REPRESENTATION_RELATIONSHIP_WITH_TRANSFORMATION(#57)
SHAPE_REPRESENTATION_RELATIONSHIP()
);
#117=(
REPRESENTATION_RELATIONSHIP($,$,#6060,#6056)
REPRESENTATION_RELATIONSHIP_WITH_TRANSFORMATION(#58)
SHAPE_REPRESENTATION_RELATIONSHIP()
);
#118=(
REPRESENTATION_RELATIONSHIP($,$,#6061,#6056)
REPRESENTATION_RELATIONSHIP_WITH_TRANSFORMATION(#59)
SHAPE_REPRESENTATION_RELATIONSHIP()
);
#119=(
REPRESENTATION_RELATIONSHIP($,$,#6040,#6039)
REPRESENTATION_RELATIONSHIP_WITH_TRANSFORMATION(#60)
SHAPE_REPRESENTATION_RELATIONSHIP()
);
#120=(
REPRESENTATION_RELATIONSHIP($,$,#6042,#6039)
REPRESENTATION_RELATIONSHIP_WITH_TRANSFORMATION(#61)
SHAPE_REPRESENTATION_RELATIONSHIP()
);
#121=(
REPRESENTATION_RELATIONSHIP($,$,#6049,#6039)
REPRESENTATION_RELATIONSHIP_WITH_TRANSFORMATION(#62)
SHAPE_REPRESENTATION_RELATIONSHIP()
);
#122=(
REPRESENTATION_RELATIONSHIP($,$,#6050,#6039)
REPRESENTATION_RELATIONSHIP_WITH_TRANSFORMATION(#63)
SHAPE_REPRESENTATION_RELATIONSHIP()
);
#123=(
REPRESENTATION_RELATIONSHIP($,$,#6051,#6039)
REPRESENTATION_RELATIONSHIP_WITH_TRANSFORMATION(#64)
SHAPE_REPRESENTATION_RELATIONSHIP()
);
#124=(
REPRESENTATION_RELATIONSHIP($,$,#6052,#6039)
REPRESENTATION_RELATIONSHIP_WITH_TRANSFORMATION(#65)
SHAPE_REPRESENTATION_RELATIONSHIP()
);
#125=(
REPRESENTATION_RELATIONSHIP($,$,#6053,#6039)
REPRESENTATION_RELATIONSHIP_WITH_TRANSFORMATION(#66)
SHAPE_REPRESENTATION_RELATIONSHIP()
);
#126=(
REPRESENTATION_RELATIONSHIP($,$,#6054,#6039)
REPRESENTATION_RELATIONSHIP_WITH_TRANSFORMATION(#67)
SHAPE_REPRESENTATION_RELATIONSHIP()
);
#127=(
REPRESENTATION_RELATIONSHIP($,$,#6056,#6039)
REPRESENTATION_RELATIONSHIP_WITH_TRANSFORMATION(#68)
SHAPE_REPRESENTATION_RELATIONSHIP()
);
#128=(
REPRESENTATION_RELATIONSHIP($,$,#6056,#6039)
REPRESENTATION_RELATIONSHIP_WITH_TRANSFORMATION(#69)
SHAPE_REPRESENTATION_RELATIONSHIP()
);
#129=CONTEXT_DEPENDENT_SHAPE_REPRESENTATION(#70,#5967);
#130=CONTEXT_DEPENDENT_SHAPE_REPRESENTATION(#71,#5968);
#131=CONTEXT_DEPENDENT_SHAPE_REPRESENTATION(#72,#5969);
#132=CONTEXT_DEPENDENT_SHAPE_REPRESENTATION(#73,#5970);
#133=CONTEXT_DEPENDENT_SHAPE_REPRESENTATION(#74,#5971);
#134=CONTEXT_DEPENDENT_SHAPE_REPRESENTATION(#75,#5972);
#135=CONTEXT_DEPENDENT_SHAPE_REPRESENTATION(#76,#5980);
#136=CONTEXT_DEPENDENT_SHAPE_REPRESENTATION(#77,#5987);
#137=CONTEXT_DEPENDENT_SHAPE_REPRESENTATION(#78,#5988);
#138=CONTEXT_DEPENDENT_SHAPE_REPRESENTATION(#79,#5989);
#139=CONTEXT_DEPENDENT_SHAPE_REPRESENTATION(#80,#5990);
#140=CONTEXT_DEPENDENT_SHAPE_REPRESENTATION(#81,#5991);
#141=CONTEXT_DEPENDENT_SHAPE_REPRESENTATION(#82,#5992);
#142=CONTEXT_DEPENDENT_SHAPE_REPRESENTATION(#83,#5993);
#143=CONTEXT_DEPENDENT_SHAPE_REPRESENTATION(#84,#5994);
#144=CONTEXT_DEPENDENT_SHAPE_REPRESENTATION(#85,#5995);
#145=CONTEXT_DEPENDENT_SHAPE_REPRESENTATION(#86,#5996);
#146=CONTEXT_DEPENDENT_SHAPE_REPRESENTATION(#87,#5997);
#147=CONTEXT_DEPENDENT_SHAPE_REPRESENTATION(#88,#5998);
#148=CONTEXT_DEPENDENT_SHAPE_REPRESENTATION(#89,#5999);
#149=CONTEXT_DEPENDENT_SHAPE_REPRESENTATION(#90,#6000);
#150=CONTEXT_DEPENDENT_SHAPE_REPRESENTATION(#91,#6001);
#151=CONTEXT_DEPENDENT_SHAPE_REPRESENTATION(#92,#6002);
#152=CONTEXT_DEPENDENT_SHAPE_REPRESENTATION(#93,#6003);
#153=CONTEXT_DEPENDENT_SHAPE_REPRESENTATION(#94,#6004);
#154=CONTEXT_DEPENDENT_SHAPE_REPRESENTATION(#95,#6005);
#155=CONTEXT_DEPENDENT_SHAPE_REPRESENTATION(#96,#6006);
#156=CONTEXT_DEPENDENT_SHAPE_REPRESENTATION(#97,#6007);
#157=CONTEXT_DEPENDENT_SHAPE_REPRESENTATION(#98,#6008);
#158=CONTEXT_DEPENDENT_SHAPE_REPRESENTATION(#99,#6009);
#159=CONTEXT_DEPENDENT_SHAPE_REPRESENTATION(#100,#6010);
#160=CONTEXT_DEPENDENT_SHAPE_REPRESENTATION(#101,#6011);
#161=CONTEXT_DEPENDENT_SHAPE_REPRESENTATION(#102,#6012);
#162=CONTEXT_DEPENDENT_SHAPE_REPRESENTATION(#103,#6013);
#163=CONTEXT_DEPENDENT_SHAPE_REPRESENTATION(#104,#6014);
#164=CONTEXT_DEPENDENT_SHAPE_REPRESENTATION(#105,#6015);
#165=CONTEXT_DEPENDENT_SHAPE_REPRESENTATION(#106,#6016);
#166=CONTEXT_DEPENDENT_SHAPE_REPRESENTATION(#107,#6017);
#167=CONTEXT_DEPENDENT_SHAPE_REPRESENTATION(#108,#6018);
#168=CONTEXT_DEPENDENT_SHAPE_REPRESENTATION(#109,#6019);
#169=CONTEXT_DEPENDENT_SHAPE_REPRESENTATION(#110,#6020);
#170=CONTEXT_DEPENDENT_SHAPE_REPRESENTATION(#111,#6021);
#171=CONTEXT_DEPENDENT_SHAPE_REPRESENTATION(#112,#6022);
#172=CONTEXT_DEPENDENT_SHAPE_REPRESENTATION(#113,#6023);
#173=CONTEXT_DEPENDENT_SHAPE_REPRESENTATION(#114,#6024);
#174=CONTEXT_DEPENDENT_SHAPE_REPRESENTATION(#115,#6025);
#175=CONTEXT_DEPENDENT_SHAPE_REPRESENTATION(#116,#6026);
#176=CONTEXT_DEPENDENT_SHAPE_REPRESENTATION(#117,#6027);
#177=CONTEXT_DEPENDENT_SHAPE_REPRESENTATION(#118,#6028);
#178=CONTEXT_DEPENDENT_SHAPE_REPRESENTATION(#119,#6029);
#179=CONTEXT_DEPENDENT_SHAPE_REPRESENTATION(#120,#6030);
#180=CONTEXT_DEPENDENT_SHAPE_REPRESENTATION(#121,#6031);
#181=CONTEXT_DEPENDENT_SHAPE_REPRESENTATION(#122,#6032);
#182=CONTEXT_DEPENDENT_SHAPE_REPRESENTATION(#123,#6033);
#183=CONTEXT_DEPENDENT_SHAPE_REPRESENTATION(#124,#6034);
#184=CONTEXT_DEPENDENT_SHAPE_REPRESENTATION(#125,#6035);
#185=CONTEXT_DEPENDENT_SHAPE_REPRESENTATION(#126,#6036);
#186=CONTEXT_DEPENDENT_SHAPE_REPRESENTATION(#127,#6037);
#187=CONTEXT_DEPENDENT_SHAPE_REPRESENTATION(#128,#6038);
#188=NEXT_ASSEMBLY_USAGE_OCCURRENCE('Offset cable chain link:1',
'Offset cable chain link:1','Offset cable chain link:1',#6066,#6067,
'Offset cable chain link:1');
#189=NEXT_ASSEMBLY_USAGE_OCCURRENCE('Hinge bearing sleeve:2',
'Hinge bearing sleeve:2','Hinge bearing sleeve:2',#6066,#6068,
'Hinge bearing sleeve:2');
#190=NEXT_ASSEMBLY_USAGE_OCCURRENCE('Forty millimetre hinge bolt:3',
'Forty millimetre hinge bolt:3','Forty millimetre hinge bolt:3',#6066,#6069,
'Forty millimetre hinge bolt:3');
#191=NEXT_ASSEMBLY_USAGE_OCCURRENCE('Flat Washer - M6:4',
'Flat Washer - M6:4','Flat Washer - M6:4',#6066,#6070,
'Flat Washer - M6:4');
#192=NEXT_ASSEMBLY_USAGE_OCCURRENCE('Flat Washer - M6:5',
'Flat Washer - M6:5','Flat Washer - M6:5',#6066,#6071,
'Flat Washer - M6:5');
#193=NEXT_ASSEMBLY_USAGE_OCCURRENCE('Hex Nut - M6:3','Hex Nut - M6:3',
'Hex Nut - M6:3',#6066,#6072,'Hex Nut - M6:3');
#194=NEXT_ASSEMBLY_USAGE_OCCURRENCE('Moving end bracket:1',
'Moving end bracket:1','Moving end bracket:1',#6078,#6079,
'Moving end bracket:1');
#195=NEXT_ASSEMBLY_USAGE_OCCURRENCE('Fixed end bracket:1',
'Fixed end bracket:1','Fixed end bracket:1',#6064,#6065,
'Fixed end bracket:1');
#196=NEXT_ASSEMBLY_USAGE_OCCURRENCE('Hinge bearing sleeve:1',
'Hinge bearing sleeve:1','Hinge bearing sleeve:1',#6064,#6082,
'Hinge bearing sleeve:1');
#197=NEXT_ASSEMBLY_USAGE_OCCURRENCE('Forty millimetre hinge bolt:2',
'Forty millimetre hinge bolt:2','Forty millimetre hinge bolt:2',#6064,#6083,
'Forty millimetre hinge bolt:2');
#198=NEXT_ASSEMBLY_USAGE_OCCURRENCE('Flat Washer - M6:2',
'Flat Washer - M6:2','Flat Washer - M6:2',#6064,#6084,
'Flat Washer - M6:2');
#199=NEXT_ASSEMBLY_USAGE_OCCURRENCE('Flat Washer - M6:3',
'Flat Washer - M6:3','Flat Washer - M6:3',#6064,#6084,
'Flat Washer - M6:3');
#200=NEXT_ASSEMBLY_USAGE_OCCURRENCE('Hex Nut - M6:2','Hex Nut - M6:2',
'Hex Nut - M6:2',#6064,#6085,'Hex Nut - M6:2');
#201=NEXT_ASSEMBLY_USAGE_OCCURRENCE('Offset cable chain link:4',
'Offset cable chain link:4','Offset cable chain link:4',#6073,#6081,
'Offset cable chain link:4');
#202=NEXT_ASSEMBLY_USAGE_OCCURRENCE('Hinge bearing sleeve:5',
'Hinge bearing sleeve:5','Hinge bearing sleeve:5',#6073,#6082,
'Hinge bearing sleeve:5');
#203=NEXT_ASSEMBLY_USAGE_OCCURRENCE('Forty millimetre hinge bolt:6',
'Forty millimetre hinge bolt:6','Forty millimetre hinge bolt:6',#6073,#6083,
'Forty millimetre hinge bolt:6');
#204=NEXT_ASSEMBLY_USAGE_OCCURRENCE('Flat Washer - M6:10',
'Flat Washer - M6:10','Flat Washer - M6:10',#6073,#6084,
'Flat Washer - M6:10');
#205=NEXT_ASSEMBLY_USAGE_OCCURRENCE('Flat Washer - M6:11',
'Flat Washer - M6:11','Flat Washer - M6:11',#6073,#6084,
'Flat Washer - M6:11');
#206=NEXT_ASSEMBLY_USAGE_OCCURRENCE('Hex Nut - M6:6','Hex Nut - M6:6',
'Hex Nut - M6:6',#6073,#6085,'Hex Nut - M6:6');
#207=NEXT_ASSEMBLY_USAGE_OCCURRENCE('Offset cable chain link:5',
'Offset cable chain link:5','Offset cable chain link:5',#6074,#6081,
'Offset cable chain link:5');
#208=NEXT_ASSEMBLY_USAGE_OCCURRENCE('Hinge bearing sleeve:6',
'Hinge bearing sleeve:6','Hinge bearing sleeve:6',#6074,#6082,
'Hinge bearing sleeve:6');
#209=NEXT_ASSEMBLY_USAGE_OCCURRENCE('Forty millimetre hinge bolt:7',
'Forty millimetre hinge bolt:7','Forty millimetre hinge bolt:7',#6074,#6083,
'Forty millimetre hinge bolt:7');
#210=NEXT_ASSEMBLY_USAGE_OCCURRENCE('Flat Washer - M6:12',
'Flat Washer - M6:12','Flat Washer - M6:12',#6074,#6084,
'Flat Washer - M6:12');
#211=NEXT_ASSEMBLY_USAGE_OCCURRENCE('Flat Washer - M6:13',
'Flat Washer - M6:13','Flat Washer - M6:13',#6074,#6084,
'Flat Washer - M6:13');
#212=NEXT_ASSEMBLY_USAGE_OCCURRENCE('Hex Nut - M6:7','Hex Nut - M6:7',
'Hex Nut - M6:7',#6074,#6085,'Hex Nut - M6:7');
#213=NEXT_ASSEMBLY_USAGE_OCCURRENCE('Offset cable chain link:6',
'Offset cable chain link:6','Offset cable chain link:6',#6075,#6081,
'Offset cable chain link:6');
#214=NEXT_ASSEMBLY_USAGE_OCCURRENCE('Hinge bearing sleeve:7',
'Hinge bearing sleeve:7','Hinge bearing sleeve:7',#6075,#6082,
'Hinge bearing sleeve:7');
#215=NEXT_ASSEMBLY_USAGE_OCCURRENCE('Forty millimetre hinge bolt:8',
'Forty millimetre hinge bolt:8','Forty millimetre hinge bolt:8',#6075,#6083,
'Forty millimetre hinge bolt:8');
#216=NEXT_ASSEMBLY_USAGE_OCCURRENCE('Flat Washer - M6:14',
'Flat Washer - M6:14','Flat Washer - M6:14',#6075,#6084,
'Flat Washer - M6:14');
#217=NEXT_ASSEMBLY_USAGE_OCCURRENCE('Flat Washer - M6:15',
'Flat Washer - M6:15','Flat Washer - M6:15',#6075,#6084,
'Flat Washer - M6:15');
#218=NEXT_ASSEMBLY_USAGE_OCCURRENCE('Hex Nut - M6:8','Hex Nut - M6:8',
'Hex Nut - M6:8',#6075,#6085,'Hex Nut - M6:8');
#219=NEXT_ASSEMBLY_USAGE_OCCURRENCE('Offset cable chain link:7',
'Offset cable chain link:7','Offset cable chain link:7',#6076,#6081,
'Offset cable chain link:7');
#220=NEXT_ASSEMBLY_USAGE_OCCURRENCE('Hinge bearing sleeve:8',
'Hinge bearing sleeve:8','Hinge bearing sleeve:8',#6076,#6082,
'Hinge bearing sleeve:8');
#221=NEXT_ASSEMBLY_USAGE_OCCURRENCE('Forty millimetre hinge bolt:9',
'Forty millimetre hinge bolt:9','Forty millimetre hinge bolt:9',#6076,#6083,
'Forty millimetre hinge bolt:9');
#222=NEXT_ASSEMBLY_USAGE_OCCURRENCE('Flat Washer - M6:16',
'Flat Washer - M6:16','Flat Washer - M6:16',#6076,#6084,
'Flat Washer - M6:16');
#223=NEXT_ASSEMBLY_USAGE_OCCURRENCE('Flat Washer - M6:17',
'Flat Washer - M6:17','Flat Washer - M6:17',#6076,#6084,
'Flat Washer - M6:17');
#224=NEXT_ASSEMBLY_USAGE_OCCURRENCE('Hex Nut - M6:9','Hex Nut - M6:9',
'Hex Nut - M6:9',#6076,#6085,'Hex Nut - M6:9');
#225=NEXT_ASSEMBLY_USAGE_OCCURRENCE('Offset cable chain link:8',
'Offset cable chain link:8','Offset cable chain link:8',#6077,#6081,
'Offset cable chain link:8');
#226=NEXT_ASSEMBLY_USAGE_OCCURRENCE('Hinge bearing sleeve:9',
'Hinge bearing sleeve:9','Hinge bearing sleeve:9',#6077,#6082,
'Hinge bearing sleeve:9');
#227=NEXT_ASSEMBLY_USAGE_OCCURRENCE('Forty millimetre hinge bolt:10',
'Forty millimetre hinge bolt:10','Forty millimetre hinge bolt:10',#6077,
#6083,'Forty millimetre hinge bolt:10');
#228=NEXT_ASSEMBLY_USAGE_OCCURRENCE('Flat Washer - M6:18',
'Flat Washer - M6:18','Flat Washer - M6:18',#6077,#6084,
'Flat Washer - M6:18');
#229=NEXT_ASSEMBLY_USAGE_OCCURRENCE('Flat Washer - M6:19',
'Flat Washer - M6:19','Flat Washer - M6:19',#6077,#6084,
'Flat Washer - M6:19');
#230=NEXT_ASSEMBLY_USAGE_OCCURRENCE('Hex Nut - M6:10','Hex Nut - M6:10',
'Hex Nut - M6:10',#6077,#6085,'Hex Nut - M6:10');
#231=NEXT_ASSEMBLY_USAGE_OCCURRENCE('Offset cable chain link:1',
'Offset cable chain link:1','Offset cable chain link:1',#6080,#6081,
'Offset cable chain link:1');
#232=NEXT_ASSEMBLY_USAGE_OCCURRENCE('Hinge bearing sleeve:2',
'Hinge bearing sleeve:2','Hinge bearing sleeve:2',#6080,#6082,
'Hinge bearing sleeve:2');
#233=NEXT_ASSEMBLY_USAGE_OCCURRENCE('Forty millimetre hinge bolt:3',
'Forty millimetre hinge bolt:3','Forty millimetre hinge bolt:3',#6080,#6083,
'Forty millimetre hinge bolt:3');
#234=NEXT_ASSEMBLY_USAGE_OCCURRENCE('Flat Washer - M6:4',
'Flat Washer - M6:4','Flat Washer - M6:4',#6080,#6084,
'Flat Washer - M6:4');
#235=NEXT_ASSEMBLY_USAGE_OCCURRENCE('Flat Washer - M6:5',
'Flat Washer - M6:5','Flat Washer - M6:5',#6080,#6084,
'Flat Washer - M6:5');
#236=NEXT_ASSEMBLY_USAGE_OCCURRENCE('Hex Nut - M6:3','Hex Nut - M6:3',
'Hex Nut - M6:3',#6080,#6085,'Hex Nut - M6:3');
#237=NEXT_ASSEMBLY_USAGE_OCCURRENCE('Fixed chain bracket:1',
'Fixed chain bracket:1','Fixed chain bracket:1',#6063,#6064,
'Fixed chain bracket:1');
#238=NEXT_ASSEMBLY_USAGE_OCCURRENCE('Cable link 1:1','Cable link 1:1',
'Cable link 1:1',#6063,#6066,'Cable link 1:1');
#239=NEXT_ASSEMBLY_USAGE_OCCURRENCE('Cable link 4:1','Cable link 4:1',
'Cable link 4:1',#6063,#6073,'Cable link 4:1');
#240=NEXT_ASSEMBLY_USAGE_OCCURRENCE('Cable link 5:1','Cable link 5:1',
'Cable link 5:1',#6063,#6074,'Cable link 5:1');
#241=NEXT_ASSEMBLY_USAGE_OCCURRENCE('Cable link 6:1','Cable link 6:1',
'Cable link 6:1',#6063,#6075,'Cable link 6:1');
#242=NEXT_ASSEMBLY_USAGE_OCCURRENCE('Cable link 7:1','Cable link 7:1',
'Cable link 7:1',#6063,#6076,'Cable link 7:1');
#243=NEXT_ASSEMBLY_USAGE_OCCURRENCE('Cable link 8:1','Cable link 8:1',
'Cable link 8:1',#6063,#6077,'Cable link 8:1');
#244=NEXT_ASSEMBLY_USAGE_OCCURRENCE('Moving chain bracket:1',
'Moving chain bracket:1','Moving chain bracket:1',#6063,#6078,
'Moving chain bracket:1');
#245=NEXT_ASSEMBLY_USAGE_OCCURRENCE('Cable link 1:2','Cable link 1:2',
'Cable link 1:2',#6063,#6080,'Cable link 1:2');
#246=NEXT_ASSEMBLY_USAGE_OCCURRENCE('Cable link 1:3','Cable link 1:3',
'Cable link 1:3',#6063,#6080,'Cable link 1:3');
#247=(
BOUNDED_CURVE()
B_SPLINE_CURVE(2,(#5191,#5192,#5193),.UNSPECIFIED.,.F.,.F.)
B_SPLINE_CURVE_WITH_KNOTS((3,3),(0.144988513094728,0.791574906712449),
 .UNSPECIFIED.)
CURVE()
GEOMETRIC_REPRESENTATION_ITEM()
RATIONAL_B_SPLINE_CURVE((1.09282032302755,1.26188021535082,1.09282032302931))
REPRESENTATION_ITEM('')
);
#248=(
BOUNDED_CURVE()
B_SPLINE_CURVE(2,(#5195,#5196,#5197),.UNSPECIFIED.,.F.,.F.)
B_SPLINE_CURVE_WITH_KNOTS((3,3),(0.144988513094728,0.791574906712449),
 .UNSPECIFIED.)
CURVE()
GEOMETRIC_REPRESENTATION_ITEM()
RATIONAL_B_SPLINE_CURVE((1.09282032302755,1.26188021535082,1.09282032302931))
REPRESENTATION_ITEM('')
);
#249=(
BOUNDED_CURVE()
B_SPLINE_CURVE(2,(#5199,#5200,#5201),.UNSPECIFIED.,.F.,.F.)
B_SPLINE_CURVE_WITH_KNOTS((3,3),(0.144988513094728,0.791574906712449),
 .UNSPECIFIED.)
CURVE()
GEOMETRIC_REPRESENTATION_ITEM()
RATIONAL_B_SPLINE_CURVE((1.09282032302755,1.26188021535082,1.09282032302931))
REPRESENTATION_ITEM('')
);
#250=(
BOUNDED_CURVE()
B_SPLINE_CURVE(2,(#5203,#5204,#5205),.UNSPECIFIED.,.F.,.F.)
B_SPLINE_CURVE_WITH_KNOTS((3,3),(0.144988513094728,0.791574906712449),
 .UNSPECIFIED.)
CURVE()
GEOMETRIC_REPRESENTATION_ITEM()
RATIONAL_B_SPLINE_CURVE((1.09282032302755,1.26188021535082,1.09282032302931))
REPRESENTATION_ITEM('')
);
#251=(
BOUNDED_CURVE()
B_SPLINE_CURVE(2,(#5207,#5208,#5209),.UNSPECIFIED.,.F.,.F.)
B_SPLINE_CURVE_WITH_KNOTS((3,3),(0.144988513094728,0.791574906712449),
 .UNSPECIFIED.)
CURVE()
GEOMETRIC_REPRESENTATION_ITEM()
RATIONAL_B_SPLINE_CURVE((1.09282032302755,1.26188021535082,1.09282032302931))
REPRESENTATION_ITEM('')
);
#252=(
BOUNDED_CURVE()
B_SPLINE_CURVE(2,(#5210,#5211,#5212),.UNSPECIFIED.,.F.,.F.)
B_SPLINE_CURVE_WITH_KNOTS((3,3),(0.144988513094727,0.791574906712449),
 .UNSPECIFIED.)
CURVE()
GEOMETRIC_REPRESENTATION_ITEM()
RATIONAL_B_SPLINE_CURVE((1.09282032302755,1.26188021535082,1.09282032302931))
REPRESENTATION_ITEM('')
);
#253=(
BOUNDED_CURVE()
B_SPLINE_CURVE(2,(#5273,#5274,#5275),.UNSPECIFIED.,.F.,.F.)
B_SPLINE_CURVE_WITH_KNOTS((3,3),(0.144988513094728,0.791574906712449),
 .UNSPECIFIED.)
CURVE()
GEOMETRIC_REPRESENTATION_ITEM()
RATIONAL_B_SPLINE_CURVE((1.09282032302755,1.26188021535082,1.09282032302931))
REPRESENTATION_ITEM('')
);
#254=(
BOUNDED_CURVE()
B_SPLINE_CURVE(2,(#5277,#5278,#5279),.UNSPECIFIED.,.F.,.F.)
B_SPLINE_CURVE_WITH_KNOTS((3,3),(0.144988513094728,0.791574906712449),
 .UNSPECIFIED.)
CURVE()
GEOMETRIC_REPRESENTATION_ITEM()
RATIONAL_B_SPLINE_CURVE((1.09282032302755,1.26188021535082,1.09282032302931))
REPRESENTATION_ITEM('')
);
#255=(
BOUNDED_CURVE()
B_SPLINE_CURVE(2,(#5284,#5285,#5286),.UNSPECIFIED.,.F.,.F.)
B_SPLINE_CURVE_WITH_KNOTS((3,3),(0.144988513094728,0.791574906712449),
 .UNSPECIFIED.)
CURVE()
GEOMETRIC_REPRESENTATION_ITEM()
RATIONAL_B_SPLINE_CURVE((1.09282032302755,1.26188021535082,1.09282032302931))
REPRESENTATION_ITEM('')
);
#256=(
BOUNDED_CURVE()
B_SPLINE_CURVE(2,(#5288,#5289,#5290),.UNSPECIFIED.,.F.,.F.)
B_SPLINE_CURVE_WITH_KNOTS((3,3),(0.144988513094728,0.791574906712449),
 .UNSPECIFIED.)
CURVE()
GEOMETRIC_REPRESENTATION_ITEM()
RATIONAL_B_SPLINE_CURVE((1.09282032302755,1.26188021535082,1.09282032302931))
REPRESENTATION_ITEM('')
);
#257=(
BOUNDED_CURVE()
B_SPLINE_CURVE(2,(#5292,#5293,#5294),.UNSPECIFIED.,.F.,.F.)
B_SPLINE_CURVE_WITH_KNOTS((3,3),(0.144988513094728,0.791574906712449),
 .UNSPECIFIED.)
CURVE()
GEOMETRIC_REPRESENTATION_ITEM()
RATIONAL_B_SPLINE_CURVE((1.09282032302755,1.26188021535082,1.09282032302931))
REPRESENTATION_ITEM('')
);
#258=(
BOUNDED_CURVE()
B_SPLINE_CURVE(2,(#5295,#5296,#5297),.UNSPECIFIED.,.F.,.F.)
B_SPLINE_CURVE_WITH_KNOTS((3,3),(0.144988513094728,0.791574906712449),
 .UNSPECIFIED.)
CURVE()
GEOMETRIC_REPRESENTATION_ITEM()
RATIONAL_B_SPLINE_CURVE((1.09282032302755,1.26188021535082,1.09282032302931))
REPRESENTATION_ITEM('')
);
#259=(
BOUNDED_CURVE()
B_SPLINE_CURVE(2,(#5304,#5305,#5306),.UNSPECIFIED.,.F.,.F.)
B_SPLINE_CURVE_WITH_KNOTS((3,3),(0.144988513094728,0.791574906712449),
 .UNSPECIFIED.)
CURVE()
GEOMETRIC_REPRESENTATION_ITEM()
RATIONAL_B_SPLINE_CURVE((1.09282032302755,1.26188021535082,1.09282032302931))
REPRESENTATION_ITEM('')
);
#260=(
BOUNDED_CURVE()
B_SPLINE_CURVE(2,(#5308,#5309,#5310),.UNSPECIFIED.,.F.,.F.)
B_SPLINE_CURVE_WITH_KNOTS((3,3),(0.144988513094727,0.791574906712449),
 .UNSPECIFIED.)
CURVE()
GEOMETRIC_REPRESENTATION_ITEM()
RATIONAL_B_SPLINE_CURVE((1.09282032302755,1.26188021535082,1.09282032302931))
REPRESENTATION_ITEM('')
);
#261=(
BOUNDED_CURVE()
B_SPLINE_CURVE(2,(#5312,#5313,#5314),.UNSPECIFIED.,.F.,.F.)
B_SPLINE_CURVE_WITH_KNOTS((3,3),(0.144988513094728,0.791574906712449),
 .UNSPECIFIED.)
CURVE()
GEOMETRIC_REPRESENTATION_ITEM()
RATIONAL_B_SPLINE_CURVE((1.09282032302755,1.26188021535082,1.09282032302931))
REPRESENTATION_ITEM('')
);
#262=(
BOUNDED_CURVE()
B_SPLINE_CURVE(2,(#5316,#5317,#5318),.UNSPECIFIED.,.F.,.F.)
B_SPLINE_CURVE_WITH_KNOTS((3,3),(0.144988513094728,0.791574906712449),
 .UNSPECIFIED.)
CURVE()
GEOMETRIC_REPRESENTATION_ITEM()
RATIONAL_B_SPLINE_CURVE((1.09282032302755,1.26188021535082,1.09282032302931))
REPRESENTATION_ITEM('')
);
#263=(
BOUNDED_CURVE()
B_SPLINE_CURVE(2,(#5320,#5321,#5322),.UNSPECIFIED.,.F.,.F.)
B_SPLINE_CURVE_WITH_KNOTS((3,3),(0.144988513094728,0.791574906712449),
 .UNSPECIFIED.)
CURVE()
GEOMETRIC_REPRESENTATION_ITEM()
RATIONAL_B_SPLINE_CURVE((1.09282032302755,1.26188021535082,1.09282032302931))
REPRESENTATION_ITEM('')
);
#264=(
BOUNDED_CURVE()
B_SPLINE_CURVE(2,(#5323,#5324,#5325),.UNSPECIFIED.,.F.,.F.)
B_SPLINE_CURVE_WITH_KNOTS((3,3),(0.144988513094727,0.791574906712449),
 .UNSPECIFIED.)
CURVE()
GEOMETRIC_REPRESENTATION_ITEM()
RATIONAL_B_SPLINE_CURVE((1.09282032302755,1.26188021535082,1.09282032302931))
REPRESENTATION_ITEM('')
);
#265=(
BOUNDED_CURVE()
B_SPLINE_CURVE(2,(#5690,#5691,#5692),.UNSPECIFIED.,.F.,.F.)
B_SPLINE_CURVE_WITH_KNOTS((3,3),(0.144988513094728,0.791574906712449),
 .UNSPECIFIED.)
CURVE()
GEOMETRIC_REPRESENTATION_ITEM()
RATIONAL_B_SPLINE_CURVE((1.09282032302755,1.26188021535082,1.09282032302931))
REPRESENTATION_ITEM('')
);
#266=(
BOUNDED_CURVE()
B_SPLINE_CURVE(2,(#5694,#5695,#5696),.UNSPECIFIED.,.F.,.F.)
B_SPLINE_CURVE_WITH_KNOTS((3,3),(0.144988513094728,0.791574906712449),
 .UNSPECIFIED.)
CURVE()
GEOMETRIC_REPRESENTATION_ITEM()
RATIONAL_B_SPLINE_CURVE((1.09282032302755,1.26188021535082,1.09282032302931))
REPRESENTATION_ITEM('')
);
#267=(
BOUNDED_CURVE()
B_SPLINE_CURVE(2,(#5698,#5699,#5700),.UNSPECIFIED.,.F.,.F.)
B_SPLINE_CURVE_WITH_KNOTS((3,3),(0.144988513094728,0.791574906712449),
 .UNSPECIFIED.)
CURVE()
GEOMETRIC_REPRESENTATION_ITEM()
RATIONAL_B_SPLINE_CURVE((1.09282032302755,1.26188021535082,1.09282032302931))
REPRESENTATION_ITEM('')
);
#268=(
BOUNDED_CURVE()
B_SPLINE_CURVE(2,(#5702,#5703,#5704),.UNSPECIFIED.,.F.,.F.)
B_SPLINE_CURVE_WITH_KNOTS((3,3),(0.144988513094728,0.791574906712449),
 .UNSPECIFIED.)
CURVE()
GEOMETRIC_REPRESENTATION_ITEM()
RATIONAL_B_SPLINE_CURVE((1.09282032302755,1.26188021535082,1.09282032302931))
REPRESENTATION_ITEM('')
);
#269=(
BOUNDED_CURVE()
B_SPLINE_CURVE(2,(#5706,#5707,#5708),.UNSPECIFIED.,.F.,.F.)
B_SPLINE_CURVE_WITH_KNOTS((3,3),(0.144988513094728,0.791574906712449),
 .UNSPECIFIED.)
CURVE()
GEOMETRIC_REPRESENTATION_ITEM()
RATIONAL_B_SPLINE_CURVE((1.09282032302755,1.26188021535082,1.09282032302931))
REPRESENTATION_ITEM('')
);
#270=(
BOUNDED_CURVE()
B_SPLINE_CURVE(2,(#5709,#5710,#5711),.UNSPECIFIED.,.F.,.F.)
B_SPLINE_CURVE_WITH_KNOTS((3,3),(0.144988513094727,0.791574906712449),
 .UNSPECIFIED.)
CURVE()
GEOMETRIC_REPRESENTATION_ITEM()
RATIONAL_B_SPLINE_CURVE((1.09282032302755,1.26188021535082,1.09282032302931))
REPRESENTATION_ITEM('')
);
#271=(
BOUNDED_CURVE()
B_SPLINE_CURVE(2,(#5757,#5758,#5759),.UNSPECIFIED.,.F.,.F.)
B_SPLINE_CURVE_WITH_KNOTS((3,3),(0.144988513094728,0.791574906712449),
 .UNSPECIFIED.)
CURVE()
GEOMETRIC_REPRESENTATION_ITEM()
RATIONAL_B_SPLINE_CURVE((1.09282032302755,1.26188021535082,1.09282032302931))
REPRESENTATION_ITEM('')
);
#272=(
BOUNDED_CURVE()
B_SPLINE_CURVE(2,(#5761,#5762,#5763),.UNSPECIFIED.,.F.,.F.)
B_SPLINE_CURVE_WITH_KNOTS((3,3),(0.144988513094728,0.791574906712449),
 .UNSPECIFIED.)
CURVE()
GEOMETRIC_REPRESENTATION_ITEM()
RATIONAL_B_SPLINE_CURVE((1.09282032302755,1.26188021535082,1.09282032302931))
REPRESENTATION_ITEM('')
);
#273=(
BOUNDED_CURVE()
B_SPLINE_CURVE(2,(#5768,#5769,#5770),.UNSPECIFIED.,.F.,.F.)
B_SPLINE_CURVE_WITH_KNOTS((3,3),(0.144988513094728,0.791574906712449),
 .UNSPECIFIED.)
CURVE()
GEOMETRIC_REPRESENTATION_ITEM()
RATIONAL_B_SPLINE_CURVE((1.09282032302755,1.26188021535082,1.09282032302931))
REPRESENTATION_ITEM('')
);
#274=(
BOUNDED_CURVE()
B_SPLINE_CURVE(2,(#5772,#5773,#5774),.UNSPECIFIED.,.F.,.F.)
B_SPLINE_CURVE_WITH_KNOTS((3,3),(0.144988513094728,0.791574906712449),
 .UNSPECIFIED.)
CURVE()
GEOMETRIC_REPRESENTATION_ITEM()
RATIONAL_B_SPLINE_CURVE((1.09282032302755,1.26188021535082,1.09282032302931))
REPRESENTATION_ITEM('')
);
#275=(
BOUNDED_CURVE()
B_SPLINE_CURVE(2,(#5776,#5777,#5778),.UNSPECIFIED.,.F.,.F.)
B_SPLINE_CURVE_WITH_KNOTS((3,3),(0.144988513094728,0.791574906712449),
 .UNSPECIFIED.)
CURVE()
GEOMETRIC_REPRESENTATION_ITEM()
RATIONAL_B_SPLINE_CURVE((1.09282032302755,1.26188021535082,1.09282032302931))
REPRESENTATION_ITEM('')
);
#276=(
BOUNDED_CURVE()
B_SPLINE_CURVE(2,(#5779,#5780,#5781),.UNSPECIFIED.,.F.,.F.)
B_SPLINE_CURVE_WITH_KNOTS((3,3),(0.144988513094728,0.791574906712449),
 .UNSPECIFIED.)
CURVE()
GEOMETRIC_REPRESENTATION_ITEM()
RATIONAL_B_SPLINE_CURVE((1.09282032302755,1.26188021535082,1.09282032302931))
REPRESENTATION_ITEM('')
);
#277=(
BOUNDED_CURVE()
B_SPLINE_CURVE(2,(#5788,#5789,#5790),.UNSPECIFIED.,.F.,.F.)
B_SPLINE_CURVE_WITH_KNOTS((3,3),(0.144988513094728,0.791574906712449),
 .UNSPECIFIED.)
CURVE()
GEOMETRIC_REPRESENTATION_ITEM()
RATIONAL_B_SPLINE_CURVE((1.09282032302755,1.26188021535082,1.09282032302931))
REPRESENTATION_ITEM('')
);
#278=(
BOUNDED_CURVE()
B_SPLINE_CURVE(2,(#5792,#5793,#5794),.UNSPECIFIED.,.F.,.F.)
B_SPLINE_CURVE_WITH_KNOTS((3,3),(0.144988513094727,0.791574906712449),
 .UNSPECIFIED.)
CURVE()
GEOMETRIC_REPRESENTATION_ITEM()
RATIONAL_B_SPLINE_CURVE((1.09282032302755,1.26188021535082,1.09282032302931))
REPRESENTATION_ITEM('')
);
#279=(
BOUNDED_CURVE()
B_SPLINE_CURVE(2,(#5796,#5797,#5798),.UNSPECIFIED.,.F.,.F.)
B_SPLINE_CURVE_WITH_KNOTS((3,3),(0.144988513094728,0.791574906712449),
 .UNSPECIFIED.)
CURVE()
GEOMETRIC_REPRESENTATION_ITEM()
RATIONAL_B_SPLINE_CURVE((1.09282032302755,1.26188021535082,1.09282032302931))
REPRESENTATION_ITEM('')
);
#280=(
BOUNDED_CURVE()
B_SPLINE_CURVE(2,(#5800,#5801,#5802),.UNSPECIFIED.,.F.,.F.)
B_SPLINE_CURVE_WITH_KNOTS((3,3),(0.144988513094728,0.791574906712449),
 .UNSPECIFIED.)
CURVE()
GEOMETRIC_REPRESENTATION_ITEM()
RATIONAL_B_SPLINE_CURVE((1.09282032302755,1.26188021535082,1.09282032302931))
REPRESENTATION_ITEM('')
);
#281=(
BOUNDED_CURVE()
B_SPLINE_CURVE(2,(#5804,#5805,#5806),.UNSPECIFIED.,.F.,.F.)
B_SPLINE_CURVE_WITH_KNOTS((3,3),(0.144988513094728,0.791574906712449),
 .UNSPECIFIED.)
CURVE()
GEOMETRIC_REPRESENTATION_ITEM()
RATIONAL_B_SPLINE_CURVE((1.09282032302755,1.26188021535082,1.09282032302931))
REPRESENTATION_ITEM('')
);
#282=(
BOUNDED_CURVE()
B_SPLINE_CURVE(2,(#5807,#5808,#5809),.UNSPECIFIED.,.F.,.F.)
B_SPLINE_CURVE_WITH_KNOTS((3,3),(0.144988513094727,0.791574906712449),
 .UNSPECIFIED.)
CURVE()
GEOMETRIC_REPRESENTATION_ITEM()
RATIONAL_B_SPLINE_CURVE((1.09282032302755,1.26188021535082,1.09282032302931))
REPRESENTATION_ITEM('')
);
#283=CONICAL_SURFACE('',#3546,0.270000000000031,0.785398163397448);
#284=CONICAL_SURFACE('',#3547,0.576175134594879,1.0471975511966);
#285=CONICAL_SURFACE('',#3576,0.576175134594879,1.0471975511966);
#286=CONICAL_SURFACE('',#3578,0.576175134594879,1.0471975511966);
#287=CONICAL_SURFACE('',#3726,0.27,0.785398163397448);
#288=CONICAL_SURFACE('',#3727,0.576175134594813,1.0471975511966);
#289=CONICAL_SURFACE('',#3747,0.576175134594813,1.0471975511966);
#290=CONICAL_SURFACE('',#3749,0.576175134594813,1.0471975511966);
#291=ELLIPSE('',#3464,0.415214835958494,0.410000000000047);
#292=ELLIPSE('',#3467,0.415214835958494,0.410000000000047);
#293=ELLIPSE('',#3473,0.415214835958495,0.410000000000047);
#294=ELLIPSE('',#3475,0.415214835958495,0.410000000000047);
#295=ELLIPSE('',#3478,0.415214835958495,0.410000000000047);
#296=ELLIPSE('',#3480,0.415214835958495,0.410000000000047);
#297=ELLIPSE('',#3486,0.708903378465722,0.70000000000008);
#298=ELLIPSE('',#3488,0.708903378465722,0.70000000000008);
#299=ELLIPSE('',#3499,0.708903378465722,0.70000000000008);
#300=ELLIPSE('',#3510,0.708903378465722,0.70000000000008);
#301=ELLIPSE('',#3644,0.415214835958447,0.41);
#302=ELLIPSE('',#3647,0.415214835958447,0.41);
#303=ELLIPSE('',#3653,0.415214835958447,0.41);
#304=ELLIPSE('',#3655,0.415214835958447,0.41);
#305=ELLIPSE('',#3658,0.415214835958447,0.41);
#306=ELLIPSE('',#3660,0.415214835958447,0.41);
#307=ELLIPSE('',#3666,0.708903378465641,0.7);
#308=ELLIPSE('',#3668,0.708903378465641,0.7);
#309=ELLIPSE('',#3679,0.708903378465641,0.7);
#310=ELLIPSE('',#3690,0.708903378465641,0.7);
#311=SHAPE_REPRESENTATION_RELATIONSHIP('SRR','None',#6041,#324);
#312=SHAPE_REPRESENTATION_RELATIONSHIP('SRR','None',#6043,#325);
#313=SHAPE_REPRESENTATION_RELATIONSHIP('SRR','None',#6044,#326);
#314=SHAPE_REPRESENTATION_RELATIONSHIP('SRR','None',#6045,#327);
#315=SHAPE_REPRESENTATION_RELATIONSHIP('SRR','None',#6046,#328);
#316=SHAPE_REPRESENTATION_RELATIONSHIP('SRR','None',#6047,#329);
#317=SHAPE_REPRESENTATION_RELATIONSHIP('SRR','None',#6048,#330);
#318=SHAPE_REPRESENTATION_RELATIONSHIP('SRR','None',#6055,#331);
#319=SHAPE_REPRESENTATION_RELATIONSHIP('SRR','None',#6057,#332);
#320=SHAPE_REPRESENTATION_RELATIONSHIP('SRR','None',#6058,#333);
#321=SHAPE_REPRESENTATION_RELATIONSHIP('SRR','None',#6059,#334);
#322=SHAPE_REPRESENTATION_RELATIONSHIP('SRR','None',#6060,#335);
#323=SHAPE_REPRESENTATION_RELATIONSHIP('SRR','None',#6061,#336);
#324=ADVANCED_BREP_SHAPE_REPRESENTATION('',(#350),#5908);
#325=ADVANCED_BREP_SHAPE_REPRESENTATION('',(#351),#5910);
#326=ADVANCED_BREP_SHAPE_REPRESENTATION('',(#352),#5911);
#327=ADVANCED_BREP_SHAPE_REPRESENTATION('',(#353),#5912);
#328=ADVANCED_BREP_SHAPE_REPRESENTATION('',(#354),#5913);
#329=ADVANCED_BREP_SHAPE_REPRESENTATION('',(#355),#5914);
#330=ADVANCED_BREP_SHAPE_REPRESENTATION('',(#356),#5915);
#331=ADVANCED_BREP_SHAPE_REPRESENTATION('',(#357),#5922);
#332=ADVANCED_BREP_SHAPE_REPRESENTATION('',(#358),#5924);
#333=ADVANCED_BREP_SHAPE_REPRESENTATION('',(#359),#5925);
#334=ADVANCED_BREP_SHAPE_REPRESENTATION('',(#360),#5926);
#335=ADVANCED_BREP_SHAPE_REPRESENTATION('',(#361),#5927);
#336=ADVANCED_BREP_SHAPE_REPRESENTATION('',(#362),#5928);
#337=STYLED_ITEM('',(#6199),#350);
#338=STYLED_ITEM('',(#6234),#351);
#339=STYLED_ITEM('',(#6220),#352);
#340=STYLED_ITEM('',(#6227),#353);
#341=STYLED_ITEM('',(#6227),#354);
#342=STYLED_ITEM('',(#6227),#355);
#343=STYLED_ITEM('',(#6227),#356);
#344=STYLED_ITEM('',(#6199),#357);
#345=STYLED_ITEM('',(#6234),#358);
#346=STYLED_ITEM('',(#6220),#359);
#347=STYLED_ITEM('',(#6227),#360);
#348=STYLED_ITEM('',(#6227),#361);
#349=STYLED_ITEM('',(#6227),#362);
#350=MANIFOLD_SOLID_BREP('Body1',#3331);
#351=MANIFOLD_SOLID_BREP('Body1',#3332);
#352=MANIFOLD_SOLID_BREP('Body1',#3333);
#353=MANIFOLD_SOLID_BREP('Body1',#3334);
#354=MANIFOLD_SOLID_BREP('Body1',#3335);
#355=MANIFOLD_SOLID_BREP('Body1',#3336);
#356=MANIFOLD_SOLID_BREP('Body1',#3337);
#357=MANIFOLD_SOLID_BREP('Body1',#3338);
#358=MANIFOLD_SOLID_BREP('Body1',#3339);
#359=MANIFOLD_SOLID_BREP('Body1',#3340);
#360=MANIFOLD_SOLID_BREP('Body1',#3341);
#361=MANIFOLD_SOLID_BREP('Body1',#3342);
#362=MANIFOLD_SOLID_BREP('Body1',#3343);
#363=FACE_BOUND('',#715,.T.);
#364=FACE_BOUND('',#718,.T.);
#365=FACE_BOUND('',#722,.T.);
#366=FACE_BOUND('',#723,.T.);
#367=FACE_BOUND('',#726,.T.);
#368=FACE_BOUND('',#729,.T.);
#369=FACE_BOUND('',#737,.T.);
#370=FACE_BOUND('',#738,.T.);
#371=FACE_BOUND('',#751,.T.);
#372=FACE_BOUND('',#762,.T.);
#373=FACE_BOUND('',#765,.T.);
#374=FACE_BOUND('',#774,.T.);
#375=FACE_BOUND('',#780,.T.);
#376=FACE_BOUND('',#782,.T.);
#377=FACE_BOUND('',#784,.T.);
#378=FACE_BOUND('',#798,.T.);
#379=FACE_BOUND('',#802,.T.);
#380=FACE_BOUND('',#804,.T.);
#381=FACE_BOUND('',#808,.T.);
#382=FACE_BOUND('',#810,.T.);
#383=FACE_BOUND('',#821,.T.);
#384=FACE_BOUND('',#823,.T.);
#385=FACE_BOUND('',#830,.T.);
#386=FACE_BOUND('',#833,.T.);
#387=FACE_BOUND('',#839,.T.);
#388=FACE_BOUND('',#842,.T.);
#389=FACE_BOUND('',#849,.T.);
#390=FACE_BOUND('',#850,.T.);
#391=FACE_BOUND('',#852,.T.);
#392=FACE_BOUND('',#853,.T.);
#393=FACE_BOUND('',#866,.T.);
#394=FACE_BOUND('',#877,.T.);
#395=FACE_BOUND('',#880,.T.);
#396=FACE_BOUND('',#889,.T.);
#397=FACE_BOUND('',#895,.T.);
#398=FACE_BOUND('',#897,.T.);
#399=FACE_BOUND('',#899,.T.);
#400=FACE_BOUND('',#913,.T.);
#401=FACE_BOUND('',#917,.T.);
#402=FACE_BOUND('',#919,.T.);
#403=FACE_BOUND('',#930,.T.);
#404=FACE_BOUND('',#932,.T.);
#405=PLANE('',#3440);
#406=PLANE('',#3441);
#407=PLANE('',#3442);
#408=PLANE('',#3443);
#409=PLANE('',#3444);
#410=PLANE('',#3445);
#411=PLANE('',#3449);
#412=PLANE('',#3450);
#413=PLANE('',#3451);
#414=PLANE('',#3452);
#415=PLANE('',#3453);
#416=PLANE('',#3454);
#417=PLANE('',#3455);
#418=PLANE('',#3456);
#419=PLANE('',#3457);
#420=PLANE('',#3458);
#421=PLANE('',#3481);
#422=PLANE('',#3483);
#423=PLANE('',#3485);
#424=PLANE('',#3487);
#425=PLANE('',#3489);
#426=PLANE('',#3490);
#427=PLANE('',#3491);
#428=PLANE('',#3492);
#429=PLANE('',#3497);
#430=PLANE('',#3500);
#431=PLANE('',#3501);
#432=PLANE('',#3502);
#433=PLANE('',#3503);
#434=PLANE('',#3508);
#435=PLANE('',#3509);
#436=PLANE('',#3511);
#437=PLANE('',#3517);
#438=PLANE('',#3518);
#439=PLANE('',#3519);
#440=PLANE('',#3520);
#441=PLANE('',#3521);
#442=PLANE('',#3522);
#443=PLANE('',#3534);
#444=PLANE('',#3535);
#445=PLANE('',#3537);
#446=PLANE('',#3542);
#447=PLANE('',#3549);
#448=PLANE('',#3550);
#449=PLANE('',#3551);
#450=PLANE('',#3552);
#451=PLANE('',#3553);
#452=PLANE('',#3554);
#453=PLANE('',#3555);
#454=PLANE('',#3556);
#455=PLANE('',#3564);
#456=PLANE('',#3565);
#457=PLANE('',#3573);
#458=PLANE('',#3574);
#459=PLANE('',#3580);
#460=PLANE('',#3581);
#461=PLANE('',#3582);
#462=PLANE('',#3586);
#463=PLANE('',#3587);
#464=PLANE('',#3588);
#465=PLANE('',#3589);
#466=PLANE('',#3590);
#467=PLANE('',#3619);
#468=PLANE('',#3620);
#469=PLANE('',#3621);
#470=PLANE('',#3622);
#471=PLANE('',#3623);
#472=PLANE('',#3624);
#473=PLANE('',#3628);
#474=PLANE('',#3629);
#475=PLANE('',#3630);
#476=PLANE('',#3631);
#477=PLANE('',#3632);
#478=PLANE('',#3633);
#479=PLANE('',#3634);
#480=PLANE('',#3635);
#481=PLANE('',#3636);
#482=PLANE('',#3637);
#483=PLANE('',#3661);
#484=PLANE('',#3663);
#485=PLANE('',#3665);
#486=PLANE('',#3667);
#487=PLANE('',#3669);
#488=PLANE('',#3670);
#489=PLANE('',#3671);
#490=PLANE('',#3672);
#491=PLANE('',#3677);
#492=PLANE('',#3680);
#493=PLANE('',#3681);
#494=PLANE('',#3682);
#495=PLANE('',#3683);
#496=PLANE('',#3688);
#497=PLANE('',#3689);
#498=PLANE('',#3691);
#499=PLANE('',#3697);
#500=PLANE('',#3698);
#501=PLANE('',#3699);
#502=PLANE('',#3700);
#503=PLANE('',#3701);
#504=PLANE('',#3702);
#505=PLANE('',#3714);
#506=PLANE('',#3715);
#507=PLANE('',#3717);
#508=PLANE('',#3722);
#509=PLANE('',#3729);
#510=PLANE('',#3730);
#511=PLANE('',#3731);
#512=PLANE('',#3732);
#513=PLANE('',#3733);
#514=PLANE('',#3734);
#515=PLANE('',#3735);
#516=PLANE('',#3736);
#517=PLANE('',#3744);
#518=PLANE('',#3745);
#519=PLANE('',#3751);
#520=PLANE('',#3752);
#521=PLANE('',#3753);
#522=PLANE('',#3757);
#523=PLANE('',#3758);
#524=PLANE('',#3759);
#525=PLANE('',#3760);
#526=PLANE('',#3761);
#527=FACE_OUTER_BOUND('',#709,.T.);
#528=FACE_OUTER_BOUND('',#710,.T.);
#529=FACE_OUTER_BOUND('',#711,.T.);
#530=FACE_OUTER_BOUND('',#712,.T.);
#531=FACE_OUTER_BOUND('',#713,.T.);
#532=FACE_OUTER_BOUND('',#714,.T.);
#533=FACE_OUTER_BOUND('',#716,.T.);
#534=FACE_OUTER_BOUND('',#717,.T.);
#535=FACE_OUTER_BOUND('',#719,.T.);
#536=FACE_OUTER_BOUND('',#720,.T.);
#537=FACE_OUTER_BOUND('',#721,.T.);
#538=FACE_OUTER_BOUND('',#724,.T.);
#539=FACE_OUTER_BOUND('',#725,.T.);
#540=FACE_OUTER_BOUND('',#727,.T.);
#541=FACE_OUTER_BOUND('',#728,.T.);
#542=FACE_OUTER_BOUND('',#730,.T.);
#543=FACE_OUTER_BOUND('',#731,.T.);
#544=FACE_OUTER_BOUND('',#732,.T.);
#545=FACE_OUTER_BOUND('',#733,.T.);
#546=FACE_OUTER_BOUND('',#734,.T.);
#547=FACE_OUTER_BOUND('',#735,.T.);
#548=FACE_OUTER_BOUND('',#736,.T.);
#549=FACE_OUTER_BOUND('',#739,.T.);
#550=FACE_OUTER_BOUND('',#740,.T.);
#551=FACE_OUTER_BOUND('',#741,.T.);
#552=FACE_OUTER_BOUND('',#742,.T.);
#553=FACE_OUTER_BOUND('',#743,.T.);
#554=FACE_OUTER_BOUND('',#744,.T.);
#555=FACE_OUTER_BOUND('',#745,.T.);
#556=FACE_OUTER_BOUND('',#746,.T.);
#557=FACE_OUTER_BOUND('',#747,.T.);
#558=FACE_OUTER_BOUND('',#748,.T.);
#559=FACE_OUTER_BOUND('',#749,.T.);
#560=FACE_OUTER_BOUND('',#750,.T.);
#561=FACE_OUTER_BOUND('',#752,.T.);
#562=FACE_OUTER_BOUND('',#753,.T.);
#563=FACE_OUTER_BOUND('',#754,.T.);
#564=FACE_OUTER_BOUND('',#755,.T.);
#565=FACE_OUTER_BOUND('',#756,.T.);
#566=FACE_OUTER_BOUND('',#757,.T.);
#567=FACE_OUTER_BOUND('',#758,.T.);
#568=FACE_OUTER_BOUND('',#759,.T.);
#569=FACE_OUTER_BOUND('',#760,.T.);
#570=FACE_OUTER_BOUND('',#761,.T.);
#571=FACE_OUTER_BOUND('',#763,.T.);
#572=FACE_OUTER_BOUND('',#764,.T.);
#573=FACE_OUTER_BOUND('',#766,.T.);
#574=FACE_OUTER_BOUND('',#767,.T.);
#575=FACE_OUTER_BOUND('',#768,.T.);
#576=FACE_OUTER_BOUND('',#769,.T.);
#577=FACE_OUTER_BOUND('',#770,.T.);
#578=FACE_OUTER_BOUND('',#771,.T.);
#579=FACE_OUTER_BOUND('',#772,.T.);
#580=FACE_OUTER_BOUND('',#773,.T.);
#581=FACE_OUTER_BOUND('',#775,.T.);
#582=FACE_OUTER_BOUND('',#776,.T.);
#583=FACE_OUTER_BOUND('',#777,.T.);
#584=FACE_OUTER_BOUND('',#778,.T.);
#585=FACE_OUTER_BOUND('',#779,.T.);
#586=FACE_OUTER_BOUND('',#781,.T.);
#587=FACE_OUTER_BOUND('',#783,.T.);
#588=FACE_OUTER_BOUND('',#785,.T.);
#589=FACE_OUTER_BOUND('',#786,.T.);
#590=FACE_OUTER_BOUND('',#787,.T.);
#591=FACE_OUTER_BOUND('',#788,.T.);
#592=FACE_OUTER_BOUND('',#789,.T.);
#593=FACE_OUTER_BOUND('',#790,.T.);
#594=FACE_OUTER_BOUND('',#791,.T.);
#595=FACE_OUTER_BOUND('',#792,.T.);
#596=FACE_OUTER_BOUND('',#793,.T.);
#597=FACE_OUTER_BOUND('',#794,.T.);
#598=FACE_OUTER_BOUND('',#795,.T.);
#599=FACE_OUTER_BOUND('',#796,.T.);
#600=FACE_OUTER_BOUND('',#797,.T.);
#601=FACE_OUTER_BOUND('',#799,.T.);
#602=FACE_OUTER_BOUND('',#800,.T.);
#603=FACE_OUTER_BOUND('',#801,.T.);
#604=FACE_OUTER_BOUND('',#803,.T.);
#605=FACE_OUTER_BOUND('',#805,.T.);
#606=FACE_OUTER_BOUND('',#806,.T.);
#607=FACE_OUTER_BOUND('',#807,.T.);
#608=FACE_OUTER_BOUND('',#809,.T.);
#609=FACE_OUTER_BOUND('',#811,.T.);
#610=FACE_OUTER_BOUND('',#812,.T.);
#611=FACE_OUTER_BOUND('',#813,.T.);
#612=FACE_OUTER_BOUND('',#814,.T.);
#613=FACE_OUTER_BOUND('',#815,.T.);
#614=FACE_OUTER_BOUND('',#816,.T.);
#615=FACE_OUTER_BOUND('',#817,.T.);
#616=FACE_OUTER_BOUND('',#818,.T.);
#617=FACE_OUTER_BOUND('',#819,.T.);
#618=FACE_OUTER_BOUND('',#820,.T.);
#619=FACE_OUTER_BOUND('',#822,.T.);
#620=FACE_OUTER_BOUND('',#824,.T.);
#621=FACE_OUTER_BOUND('',#825,.T.);
#622=FACE_OUTER_BOUND('',#826,.T.);
#623=FACE_OUTER_BOUND('',#827,.T.);
#624=FACE_OUTER_BOUND('',#828,.T.);
#625=FACE_OUTER_BOUND('',#829,.T.);
#626=FACE_OUTER_BOUND('',#831,.T.);
#627=FACE_OUTER_BOUND('',#832,.T.);
#628=FACE_OUTER_BOUND('',#834,.T.);
#629=FACE_OUTER_BOUND('',#835,.T.);
#630=FACE_OUTER_BOUND('',#836,.T.);
#631=FACE_OUTER_BOUND('',#837,.T.);
#632=FACE_OUTER_BOUND('',#838,.T.);
#633=FACE_OUTER_BOUND('',#840,.T.);
#634=FACE_OUTER_BOUND('',#841,.T.);
#635=FACE_OUTER_BOUND('',#843,.T.);
#636=FACE_OUTER_BOUND('',#844,.T.);
#637=FACE_OUTER_BOUND('',#845,.T.);
#638=FACE_OUTER_BOUND('',#846,.T.);
#639=FACE_OUTER_BOUND('',#847,.T.);
#640=FACE_OUTER_BOUND('',#848,.T.);
#641=FACE_OUTER_BOUND('',#851,.T.);
#642=FACE_OUTER_BOUND('',#854,.T.);
#643=FACE_OUTER_BOUND('',#855,.T.);
#644=FACE_OUTER_BOUND('',#856,.T.);
#645=FACE_OUTER_BOUND('',#857,.T.);
#646=FACE_OUTER_BOUND('',#858,.T.);
#647=FACE_OUTER_BOUND('',#859,.T.);
#648=FACE_OUTER_BOUND('',#860,.T.);
#649=FACE_OUTER_BOUND('',#861,.T.);
#650=FACE_OUTER_BOUND('',#862,.T.);
#651=FACE_OUTER_BOUND('',#863,.T.);
#652=FACE_OUTER_BOUND('',#864,.T.);
#653=FACE_OUTER_BOUND('',#865,.T.);
#654=FACE_OUTER_BOUND('',#867,.T.);
#655=FACE_OUTER_BOUND('',#868,.T.);
#656=FACE_OUTER_BOUND('',#869,.T.);
#657=FACE_OUTER_BOUND('',#870,.T.);
#658=FACE_OUTER_BOUND('',#871,.T.);
#659=FACE_OUTER_BOUND('',#872,.T.);
#660=FACE_OUTER_BOUND('',#873,.T.);
#661=FACE_OUTER_BOUND('',#874,.T.);
#662=FACE_OUTER_BOUND('',#875,.T.);
#663=FACE_OUTER_BOUND('',#876,.T.);
#664=FACE_OUTER_BOUND('',#878,.T.);
#665=FACE_OUTER_BOUND('',#879,.T.);
#666=FACE_OUTER_BOUND('',#881,.T.);
#667=FACE_OUTER_BOUND('',#882,.T.);
#668=FACE_OUTER_BOUND('',#883,.T.);
#669=FACE_OUTER_BOUND('',#884,.T.);
#670=FACE_OUTER_BOUND('',#885,.T.);
#671=FACE_OUTER_BOUND('',#886,.T.);
#672=FACE_OUTER_BOUND('',#887,.T.);
#673=FACE_OUTER_BOUND('',#888,.T.);
#674=FACE_OUTER_BOUND('',#890,.T.);
#675=FACE_OUTER_BOUND('',#891,.T.);
#676=FACE_OUTER_BOUND('',#892,.T.);
#677=FACE_OUTER_BOUND('',#893,.T.);
#678=FACE_OUTER_BOUND('',#894,.T.);
#679=FACE_OUTER_BOUND('',#896,.T.);
#680=FACE_OUTER_BOUND('',#898,.T.);
#681=FACE_OUTER_BOUND('',#900,.T.);
#682=FACE_OUTER_BOUND('',#901,.T.);
#683=FACE_OUTER_BOUND('',#902,.T.);
#684=FACE_OUTER_BOUND('',#903,.T.);
#685=FACE_OUTER_BOUND('',#904,.T.);
#686=FACE_OUTER_BOUND('',#905,.T.);
#687=FACE_OUTER_BOUND('',#906,.T.);
#688=FACE_OUTER_BOUND('',#907,.T.);
#689=FACE_OUTER_BOUND('',#908,.T.);
#690=FACE_OUTER_BOUND('',#909,.T.);
#691=FACE_OUTER_BOUND('',#910,.T.);
#692=FACE_OUTER_BOUND('',#911,.T.);
#693=FACE_OUTER_BOUND('',#912,.T.);
#694=FACE_OUTER_BOUND('',#914,.T.);
#695=FACE_OUTER_BOUND('',#915,.T.);
#696=FACE_OUTER_BOUND('',#916,.T.);
#697=FACE_OUTER_BOUND('',#918,.T.);
#698=FACE_OUTER_BOUND('',#920,.T.);
#699=FACE_OUTER_BOUND('',#921,.T.);
#700=FACE_OUTER_BOUND('',#922,.T.);
#701=FACE_OUTER_BOUND('',#923,.T.);
#702=FACE_OUTER_BOUND('',#924,.T.);
#703=FACE_OUTER_BOUND('',#925,.T.);
#704=FACE_OUTER_BOUND('',#926,.T.);
#705=FACE_OUTER_BOUND('',#927,.T.);
#706=FACE_OUTER_BOUND('',#928,.T.);
#707=FACE_OUTER_BOUND('',#929,.T.);
#708=FACE_OUTER_BOUND('',#931,.T.);
#709=EDGE_LOOP('',(#2249,#2250,#2251,#2252));
#710=EDGE_LOOP('',(#2253,#2254,#2255,#2256));
#711=EDGE_LOOP('',(#2257,#2258,#2259,#2260));
#712=EDGE_LOOP('',(#2261,#2262,#2263,#2264));
#713=EDGE_LOOP('',(#2265,#2266,#2267,#2268));
#714=EDGE_LOOP('',(#2269,#2270,#2271,#2272,#2273,#2274));
#715=EDGE_LOOP('',(#2275));
#716=EDGE_LOOP('',(#2276,#2277,#2278,#2279));
#717=EDGE_LOOP('',(#2280,#2281,#2282,#2283,#2284,#2285));
#718=EDGE_LOOP('',(#2286));
#719=EDGE_LOOP('',(#2287,#2288,#2289,#2290));
#720=EDGE_LOOP('',(#2291,#2292,#2293,#2294));
#721=EDGE_LOOP('',(#2295,#2296,#2297,#2298,#2299,#2300,#2301,#2302,#2303,
#2304,#2305,#2306));
#722=EDGE_LOOP('',(#2307));
#723=EDGE_LOOP('',(#2308));
#724=EDGE_LOOP('',(#2309,#2310,#2311,#2312));
#725=EDGE_LOOP('',(#2313,#2314,#2315,#2316,#2317,#2318));
#726=EDGE_LOOP('',(#2319));
#727=EDGE_LOOP('',(#2320,#2321,#2322,#2323));
#728=EDGE_LOOP('',(#2324,#2325,#2326,#2327,#2328,#2329));
#729=EDGE_LOOP('',(#2330));
#730=EDGE_LOOP('',(#2331,#2332,#2333,#2334));
#731=EDGE_LOOP('',(#2335,#2336,#2337,#2338));
#732=EDGE_LOOP('',(#2339,#2340,#2341,#2342));
#733=EDGE_LOOP('',(#2343,#2344,#2345,#2346,#2347,#2348,#2349,#2350,#2351,
#2352,#2353,#2354));
#734=EDGE_LOOP('',(#2355,#2356,#2357,#2358));
#735=EDGE_LOOP('',(#2359,#2360,#2361,#2362));
#736=EDGE_LOOP('',(#2363,#2364,#2365,#2366));
#737=EDGE_LOOP('',(#2367));
#738=EDGE_LOOP('',(#2368));
#739=EDGE_LOOP('',(#2369,#2370,#2371,#2372,#2373,#2374));
#740=EDGE_LOOP('',(#2375,#2376,#2377,#2378,#2379,#2380));
#741=EDGE_LOOP('',(#2381,#2382,#2383,#2384,#2385,#2386));
#742=EDGE_LOOP('',(#2387,#2388,#2389,#2390,#2391,#2392));
#743=EDGE_LOOP('',(#2393,#2394,#2395,#2396,#2397));
#744=EDGE_LOOP('',(#2398,#2399,#2400,#2401,#2402));
#745=EDGE_LOOP('',(#2403,#2404,#2405,#2406,#2407,#2408,#2409,#2410,#2411));
#746=EDGE_LOOP('',(#2412,#2413,#2414,#2415,#2416,#2417,#2418,#2419,#2420));
#747=EDGE_LOOP('',(#2421,#2422,#2423,#2424));
#748=EDGE_LOOP('',(#2425,#2426,#2427,#2428));
#749=EDGE_LOOP('',(#2429,#2430,#2431,#2432));
#750=EDGE_LOOP('',(#2433,#2434));
#751=EDGE_LOOP('',(#2435));
#752=EDGE_LOOP('',(#2436,#2437,#2438,#2439));
#753=EDGE_LOOP('',(#2440,#2441,#2442,#2443));
#754=EDGE_LOOP('',(#2444,#2445));
#755=EDGE_LOOP('',(#2446,#2447,#2448,#2449,#2450,#2451,#2452,#2453,#2454,
#2455,#2456,#2457));
#756=EDGE_LOOP('',(#2458,#2459,#2460,#2461));
#757=EDGE_LOOP('',(#2462,#2463,#2464,#2465));
#758=EDGE_LOOP('',(#2466,#2467,#2468,#2469));
#759=EDGE_LOOP('',(#2470,#2471));
#760=EDGE_LOOP('',(#2472,#2473,#2474,#2475));
#761=EDGE_LOOP('',(#2476,#2477));
#762=EDGE_LOOP('',(#2478));
#763=EDGE_LOOP('',(#2479,#2480,#2481,#2482,#2483,#2484,#2485,#2486,#2487,
#2488,#2489,#2490));
#764=EDGE_LOOP('',(#2491,#2492));
#765=EDGE_LOOP('',(#2493));
#766=EDGE_LOOP('',(#2494,#2495));
#767=EDGE_LOOP('',(#2496,#2497,#2498,#2499));
#768=EDGE_LOOP('',(#2500,#2501,#2502,#2503));
#769=EDGE_LOOP('',(#2504,#2505,#2506,#2507));
#770=EDGE_LOOP('',(#2508,#2509,#2510,#2511));
#771=EDGE_LOOP('',(#2512,#2513,#2514,#2515));
#772=EDGE_LOOP('',(#2516,#2517,#2518,#2519,#2520,#2521,#2522,#2523,#2524,
#2525,#2526,#2527));
#773=EDGE_LOOP('',(#2528,#2529));
#774=EDGE_LOOP('',(#2530));
#775=EDGE_LOOP('',(#2531,#2532));
#776=EDGE_LOOP('',(#2533,#2534,#2535,#2536));
#777=EDGE_LOOP('',(#2537,#2538,#2539,#2540));
#778=EDGE_LOOP('',(#2541,#2542,#2543,#2544));
#779=EDGE_LOOP('',(#2545));
#780=EDGE_LOOP('',(#2546));
#781=EDGE_LOOP('',(#2547));
#782=EDGE_LOOP('',(#2548));
#783=EDGE_LOOP('',(#2549));
#784=EDGE_LOOP('',(#2550));
#785=EDGE_LOOP('',(#2551,#2552,#2553,#2554));
#786=EDGE_LOOP('',(#2555));
#787=EDGE_LOOP('',(#2556,#2557,#2558,#2559));
#788=EDGE_LOOP('',(#2560,#2561,#2562,#2563));
#789=EDGE_LOOP('',(#2564,#2565,#2566,#2567,#2568,#2569,#2570,#2571,#2572));
#790=EDGE_LOOP('',(#2573,#2574,#2575,#2576));
#791=EDGE_LOOP('',(#2577,#2578,#2579,#2580));
#792=EDGE_LOOP('',(#2581,#2582,#2583,#2584));
#793=EDGE_LOOP('',(#2585,#2586,#2587,#2588));
#794=EDGE_LOOP('',(#2589,#2590,#2591,#2592));
#795=EDGE_LOOP('',(#2593,#2594,#2595,#2596));
#796=EDGE_LOOP('',(#2597));
#797=EDGE_LOOP('',(#2598,#2599,#2600,#2601,#2602,#2603));
#798=EDGE_LOOP('',(#2604));
#799=EDGE_LOOP('',(#2605,#2606,#2607,#2608));
#800=EDGE_LOOP('',(#2609,#2610,#2611,#2612));
#801=EDGE_LOOP('',(#2613));
#802=EDGE_LOOP('',(#2614));
#803=EDGE_LOOP('',(#2615));
#804=EDGE_LOOP('',(#2616));
#805=EDGE_LOOP('',(#2617,#2618,#2619,#2620));
#806=EDGE_LOOP('',(#2621,#2622,#2623,#2624));
#807=EDGE_LOOP('',(#2625));
#808=EDGE_LOOP('',(#2626));
#809=EDGE_LOOP('',(#2627));
#810=EDGE_LOOP('',(#2628));
#811=EDGE_LOOP('',(#2629,#2630,#2631,#2632,#2633,#2634,#2635,#2636,#2637));
#812=EDGE_LOOP('',(#2638,#2639,#2640,#2641,#2642,#2643,#2644,#2645,#2646));
#813=EDGE_LOOP('',(#2647,#2648,#2649,#2650));
#814=EDGE_LOOP('',(#2651,#2652,#2653,#2654));
#815=EDGE_LOOP('',(#2655,#2656,#2657,#2658));
#816=EDGE_LOOP('',(#2659,#2660,#2661,#2662));
#817=EDGE_LOOP('',(#2663,#2664,#2665,#2666));
#818=EDGE_LOOP('',(#2667,#2668,#2669,#2670));
#819=EDGE_LOOP('',(#2671,#2672,#2673,#2674));
#820=EDGE_LOOP('',(#2675));
#821=EDGE_LOOP('',(#2676));
#822=EDGE_LOOP('',(#2677));
#823=EDGE_LOOP('',(#2678));
#824=EDGE_LOOP('',(#2679,#2680,#2681,#2682));
#825=EDGE_LOOP('',(#2683,#2684,#2685,#2686));
#826=EDGE_LOOP('',(#2687,#2688,#2689,#2690));
#827=EDGE_LOOP('',(#2691,#2692,#2693,#2694));
#828=EDGE_LOOP('',(#2695,#2696,#2697,#2698));
#829=EDGE_LOOP('',(#2699,#2700,#2701,#2702,#2703,#2704));
#830=EDGE_LOOP('',(#2705));
#831=EDGE_LOOP('',(#2706,#2707,#2708,#2709));
#832=EDGE_LOOP('',(#2710,#2711,#2712,#2713,#2714,#2715));
#833=EDGE_LOOP('',(#2716));
#834=EDGE_LOOP('',(#2717,#2718,#2719,#2720));
#835=EDGE_LOOP('',(#2721,#2722,#2723,#2724));
#836=EDGE_LOOP('',(#2725,#2726,#2727,#2728,#2729,#2730,#2731,#2732,#2733,
#2734,#2735,#2736));
#837=EDGE_LOOP('',(#2737,#2738,#2739,#2740));
#838=EDGE_LOOP('',(#2741,#2742,#2743,#2744,#2745,#2746));
#839=EDGE_LOOP('',(#2747));
#840=EDGE_LOOP('',(#2748,#2749,#2750,#2751));
#841=EDGE_LOOP('',(#2752,#2753,#2754,#2755,#2756,#2757));
#842=EDGE_LOOP('',(#2758));
#843=EDGE_LOOP('',(#2759,#2760,#2761,#2762));
#844=EDGE_LOOP('',(#2763,#2764,#2765,#2766));
#845=EDGE_LOOP('',(#2767,#2768,#2769,#2770));
#846=EDGE_LOOP('',(#2771,#2772,#2773,#2774));
#847=EDGE_LOOP('',(#2775,#2776,#2777,#2778));
#848=EDGE_LOOP('',(#2779,#2780,#2781,#2782,#2783,#2784,#2785,#2786,#2787,
#2788,#2789,#2790));
#849=EDGE_LOOP('',(#2791));
#850=EDGE_LOOP('',(#2792));
#851=EDGE_LOOP('',(#2793,#2794,#2795,#2796));
#852=EDGE_LOOP('',(#2797));
#853=EDGE_LOOP('',(#2798));
#854=EDGE_LOOP('',(#2799,#2800,#2801,#2802,#2803,#2804));
#855=EDGE_LOOP('',(#2805,#2806,#2807,#2808,#2809,#2810));
#856=EDGE_LOOP('',(#2811,#2812,#2813,#2814,#2815,#2816));
#857=EDGE_LOOP('',(#2817,#2818,#2819,#2820,#2821,#2822));
#858=EDGE_LOOP('',(#2823,#2824,#2825,#2826,#2827));
#859=EDGE_LOOP('',(#2828,#2829,#2830,#2831,#2832));
#860=EDGE_LOOP('',(#2833,#2834,#2835,#2836,#2837,#2838,#2839,#2840,#2841));
#861=EDGE_LOOP('',(#2842,#2843,#2844,#2845,#2846,#2847,#2848,#2849,#2850));
#862=EDGE_LOOP('',(#2851,#2852,#2853,#2854));
#863=EDGE_LOOP('',(#2855,#2856,#2857,#2858));
#864=EDGE_LOOP('',(#2859,#2860,#2861,#2862));
#865=EDGE_LOOP('',(#2863,#2864));
#866=EDGE_LOOP('',(#2865));
#867=EDGE_LOOP('',(#2866,#2867,#2868,#2869));
#868=EDGE_LOOP('',(#2870,#2871,#2872,#2873));
#869=EDGE_LOOP('',(#2874,#2875));
#870=EDGE_LOOP('',(#2876,#2877,#2878,#2879,#2880,#2881,#2882,#2883,#2884,
#2885,#2886,#2887));
#871=EDGE_LOOP('',(#2888,#2889,#2890,#2891));
#872=EDGE_LOOP('',(#2892,#2893,#2894,#2895));
#873=EDGE_LOOP('',(#2896,#2897,#2898,#2899));
#874=EDGE_LOOP('',(#2900,#2901));
#875=EDGE_LOOP('',(#2902,#2903,#2904,#2905));
#876=EDGE_LOOP('',(#2906,#2907));
#877=EDGE_LOOP('',(#2908));
#878=EDGE_LOOP('',(#2909,#2910,#2911,#2912,#2913,#2914,#2915,#2916,#2917,
#2918,#2919,#2920));
#879=EDGE_LOOP('',(#2921,#2922));
#880=EDGE_LOOP('',(#2923));
#881=EDGE_LOOP('',(#2924,#2925));
#882=EDGE_LOOP('',(#2926,#2927,#2928,#2929));
#883=EDGE_LOOP('',(#2930,#2931,#2932,#2933));
#884=EDGE_LOOP('',(#2934,#2935,#2936,#2937));
#885=EDGE_LOOP('',(#2938,#2939,#2940,#2941));
#886=EDGE_LOOP('',(#2942,#2943,#2944,#2945));
#887=EDGE_LOOP('',(#2946,#2947,#2948,#2949,#2950,#2951,#2952,#2953,#2954,
#2955,#2956,#2957));
#888=EDGE_LOOP('',(#2958,#2959));
#889=EDGE_LOOP('',(#2960));
#890=EDGE_LOOP('',(#2961,#2962));
#891=EDGE_LOOP('',(#2963,#2964,#2965,#2966));
#892=EDGE_LOOP('',(#2967,#2968,#2969,#2970));
#893=EDGE_LOOP('',(#2971,#2972,#2973,#2974));
#894=EDGE_LOOP('',(#2975));
#895=EDGE_LOOP('',(#2976));
#896=EDGE_LOOP('',(#2977));
#897=EDGE_LOOP('',(#2978));
#898=EDGE_LOOP('',(#2979));
#899=EDGE_LOOP('',(#2980));
#900=EDGE_LOOP('',(#2981,#2982,#2983,#2984));
#901=EDGE_LOOP('',(#2985));
#902=EDGE_LOOP('',(#2986,#2987,#2988,#2989));
#903=EDGE_LOOP('',(#2990,#2991,#2992,#2993));
#904=EDGE_LOOP('',(#2994,#2995,#2996,#2997,#2998,#2999,#3000,#3001,#3002));
#905=EDGE_LOOP('',(#3003,#3004,#3005,#3006));
#906=EDGE_LOOP('',(#3007,#3008,#3009,#3010));
#907=EDGE_LOOP('',(#3011,#3012,#3013,#3014));
#908=EDGE_LOOP('',(#3015,#3016,#3017,#3018));
#909=EDGE_LOOP('',(#3019,#3020,#3021,#3022));
#910=EDGE_LOOP('',(#3023,#3024,#3025,#3026));
#911=EDGE_LOOP('',(#3027));
#912=EDGE_LOOP('',(#3028,#3029,#3030,#3031,#3032,#3033));
#913=EDGE_LOOP('',(#3034));
#914=EDGE_LOOP('',(#3035,#3036,#3037,#3038));
#915=EDGE_LOOP('',(#3039,#3040,#3041,#3042));
#916=EDGE_LOOP('',(#3043));
#917=EDGE_LOOP('',(#3044));
#918=EDGE_LOOP('',(#3045));
#919=EDGE_LOOP('',(#3046));
#920=EDGE_LOOP('',(#3047,#3048,#3049,#3050,#3051,#3052,#3053,#3054,#3055));
#921=EDGE_LOOP('',(#3056,#3057,#3058,#3059,#3060,#3061,#3062,#3063,#3064));
#922=EDGE_LOOP('',(#3065,#3066,#3067,#3068));
#923=EDGE_LOOP('',(#3069,#3070,#3071,#3072));
#924=EDGE_LOOP('',(#3073,#3074,#3075,#3076));
#925=EDGE_LOOP('',(#3077,#3078,#3079,#3080));
#926=EDGE_LOOP('',(#3081,#3082,#3083,#3084));
#927=EDGE_LOOP('',(#3085,#3086,#3087,#3088));
#928=EDGE_LOOP('',(#3089,#3090,#3091,#3092));
#929=EDGE_LOOP('',(#3093));
#930=EDGE_LOOP('',(#3094));
#931=EDGE_LOOP('',(#3095));
#932=EDGE_LOOP('',(#3096));
#933=LINE('',#4865,#1193);
#934=LINE('',#4871,#1194);
#935=LINE('',#4877,#1195);
#936=LINE('',#4883,#1196);
#937=LINE('',#4888,#1197);
#938=LINE('',#4892,#1198);
#939=LINE('',#4896,#1199);
#940=LINE('',#4898,#1200);
#941=LINE('',#4900,#1201);
#942=LINE('',#4902,#1202);
#943=LINE('',#4903,#1203);
#944=LINE('',#4906,#1204);
#945=LINE('',#4907,#1205);
#946=LINE('',#4910,#1206);
#947=LINE('',#4912,#1207);
#948=LINE('',#4914,#1208);
#949=LINE('',#4915,#1209);
#950=LINE('',#4917,#1210);
#951=LINE('',#4919,#1211);
#952=LINE('',#4922,#1212);
#953=LINE('',#4924,#1213);
#954=LINE('',#4926,#1214);
#955=LINE('',#4928,#1215);
#956=LINE('',#4930,#1216);
#957=LINE('',#4932,#1217);
#958=LINE('',#4934,#1218);
#959=LINE('',#4936,#1219);
#960=LINE('',#4937,#1220);
#961=LINE('',#4941,#1221);
#962=LINE('',#4945,#1222);
#963=LINE('',#4949,#1223);
#964=LINE('',#4951,#1224);
#965=LINE('',#4952,#1225);
#966=LINE('',#4953,#1226);
#967=LINE('',#4956,#1227);
#968=LINE('',#4957,#1228);
#969=LINE('',#4959,#1229);
#970=LINE('',#4961,#1230);
#971=LINE('',#4962,#1231);
#972=LINE('',#4964,#1232);
#973=LINE('',#4969,#1233);
#974=LINE('',#4970,#1234);
#975=LINE('',#4971,#1235);
#976=LINE('',#4974,#1236);
#977=LINE('',#4975,#1237);
#978=LINE('',#4978,#1238);
#979=LINE('',#4979,#1239);
#980=LINE('',#4981,#1240);
#981=LINE('',#4989,#1241);
#982=LINE('',#5002,#1242);
#983=LINE('',#5012,#1243);
#984=LINE('',#5019,#1244);
#985=LINE('',#5027,#1245);
#986=LINE('',#5030,#1246);
#987=LINE('',#5033,#1247);
#988=LINE('',#5036,#1248);
#989=LINE('',#5039,#1249);
#990=LINE('',#5041,#1250);
#991=LINE('',#5043,#1251);
#992=LINE('',#5045,#1252);
#993=LINE('',#5049,#1253);
#994=LINE('',#5050,#1254);
#995=LINE('',#5053,#1255);
#996=LINE('',#5055,#1256);
#997=LINE('',#5059,#1257);
#998=LINE('',#5061,#1258);
#999=LINE('',#5063,#1259);
#1000=LINE('',#5064,#1260);
#1001=LINE('',#5068,#1261);
#1002=LINE('',#5070,#1262);
#1003=LINE('',#5072,#1263);
#1004=LINE('',#5073,#1264);
#1005=LINE('',#5077,#1265);
#1006=LINE('',#5079,#1266);
#1007=LINE('',#5081,#1267);
#1008=LINE('',#5082,#1268);
#1009=LINE('',#5084,#1269);
#1010=LINE('',#5085,#1270);
#1011=LINE('',#5092,#1271);
#1012=LINE('',#5094,#1272);
#1013=LINE('',#5100,#1273);
#1014=LINE('',#5101,#1274);
#1015=LINE('',#5103,#1275);
#1016=LINE('',#5104,#1276);
#1017=LINE('',#5105,#1277);
#1018=LINE('',#5107,#1278);
#1019=LINE('',#5109,#1279);
#1020=LINE('',#5110,#1280);
#1021=LINE('',#5112,#1281);
#1022=LINE('',#5120,#1282);
#1023=LINE('',#5124,#1283);
#1024=LINE('',#5125,#1284);
#1025=LINE('',#5127,#1285);
#1026=LINE('',#5128,#1286);
#1027=LINE('',#5134,#1287);
#1028=LINE('',#5135,#1288);
#1029=LINE('',#5139,#1289);
#1030=LINE('',#5141,#1290);
#1031=LINE('',#5142,#1291);
#1032=LINE('',#5144,#1292);
#1033=LINE('',#5156,#1293);
#1034=LINE('',#5162,#1294);
#1035=LINE('',#5174,#1295);
#1036=LINE('',#5181,#1296);
#1037=LINE('',#5184,#1297);
#1038=LINE('',#5189,#1298);
#1039=LINE('',#5215,#1299);
#1040=LINE('',#5217,#1300);
#1041=LINE('',#5218,#1301);
#1042=LINE('',#5221,#1302);
#1043=LINE('',#5222,#1303);
#1044=LINE('',#5225,#1304);
#1045=LINE('',#5226,#1305);
#1046=LINE('',#5229,#1306);
#1047=LINE('',#5230,#1307);
#1048=LINE('',#5233,#1308);
#1049=LINE('',#5234,#1309);
#1050=LINE('',#5236,#1310);
#1051=LINE('',#5244,#1311);
#1052=LINE('',#5250,#1312);
#1053=LINE('',#5259,#1313);
#1054=LINE('',#5265,#1314);
#1055=LINE('',#5281,#1315);
#1056=LINE('',#5302,#1316);
#1057=LINE('',#5327,#1317);
#1058=LINE('',#5328,#1318);
#1059=LINE('',#5330,#1319);
#1060=LINE('',#5332,#1320);
#1061=LINE('',#5337,#1321);
#1062=LINE('',#5340,#1322);
#1063=LINE('',#5342,#1323);
#1064=LINE('',#5363,#1324);
#1065=LINE('',#5369,#1325);
#1066=LINE('',#5375,#1326);
#1067=LINE('',#5381,#1327);
#1068=LINE('',#5386,#1328);
#1069=LINE('',#5390,#1329);
#1070=LINE('',#5394,#1330);
#1071=LINE('',#5396,#1331);
#1072=LINE('',#5398,#1332);
#1073=LINE('',#5400,#1333);
#1074=LINE('',#5401,#1334);
#1075=LINE('',#5404,#1335);
#1076=LINE('',#5405,#1336);
#1077=LINE('',#5408,#1337);
#1078=LINE('',#5410,#1338);
#1079=LINE('',#5412,#1339);
#1080=LINE('',#5413,#1340);
#1081=LINE('',#5415,#1341);
#1082=LINE('',#5417,#1342);
#1083=LINE('',#5420,#1343);
#1084=LINE('',#5422,#1344);
#1085=LINE('',#5424,#1345);
#1086=LINE('',#5426,#1346);
#1087=LINE('',#5428,#1347);
#1088=LINE('',#5430,#1348);
#1089=LINE('',#5432,#1349);
#1090=LINE('',#5434,#1350);
#1091=LINE('',#5435,#1351);
#1092=LINE('',#5439,#1352);
#1093=LINE('',#5443,#1353);
#1094=LINE('',#5447,#1354);
#1095=LINE('',#5448,#1355);
#1096=LINE('',#5450,#1356);
#1097=LINE('',#5451,#1357);
#1098=LINE('',#5454,#1358);
#1099=LINE('',#5455,#1359);
#1100=LINE('',#5458,#1360);
#1101=LINE('',#5459,#1361);
#1102=LINE('',#5460,#1362);
#1103=LINE('',#5462,#1363);
#1104=LINE('',#5466,#1364);
#1105=LINE('',#5468,#1365);
#1106=LINE('',#5469,#1366);
#1107=LINE('',#5472,#1367);
#1108=LINE('',#5474,#1368);
#1109=LINE('',#5475,#1369);
#1110=LINE('',#5477,#1370);
#1111=LINE('',#5478,#1371);
#1112=LINE('',#5488,#1372);
#1113=LINE('',#5501,#1373);
#1114=LINE('',#5511,#1374);
#1115=LINE('',#5518,#1375);
#1116=LINE('',#5526,#1376);
#1117=LINE('',#5529,#1377);
#1118=LINE('',#5532,#1378);
#1119=LINE('',#5535,#1379);
#1120=LINE('',#5538,#1380);
#1121=LINE('',#5540,#1381);
#1122=LINE('',#5542,#1382);
#1123=LINE('',#5544,#1383);
#1124=LINE('',#5548,#1384);
#1125=LINE('',#5549,#1385);
#1126=LINE('',#5552,#1386);
#1127=LINE('',#5554,#1387);
#1128=LINE('',#5558,#1388);
#1129=LINE('',#5560,#1389);
#1130=LINE('',#5562,#1390);
#1131=LINE('',#5563,#1391);
#1132=LINE('',#5567,#1392);
#1133=LINE('',#5569,#1393);
#1134=LINE('',#5571,#1394);
#1135=LINE('',#5572,#1395);
#1136=LINE('',#5576,#1396);
#1137=LINE('',#5578,#1397);
#1138=LINE('',#5580,#1398);
#1139=LINE('',#5581,#1399);
#1140=LINE('',#5583,#1400);
#1141=LINE('',#5584,#1401);
#1142=LINE('',#5591,#1402);
#1143=LINE('',#5593,#1403);
#1144=LINE('',#5599,#1404);
#1145=LINE('',#5600,#1405);
#1146=LINE('',#5602,#1406);
#1147=LINE('',#5603,#1407);
#1148=LINE('',#5604,#1408);
#1149=LINE('',#5606,#1409);
#1150=LINE('',#5608,#1410);
#1151=LINE('',#5609,#1411);
#1152=LINE('',#5611,#1412);
#1153=LINE('',#5619,#1413);
#1154=LINE('',#5623,#1414);
#1155=LINE('',#5624,#1415);
#1156=LINE('',#5626,#1416);
#1157=LINE('',#5627,#1417);
#1158=LINE('',#5633,#1418);
#1159=LINE('',#5634,#1419);
#1160=LINE('',#5638,#1420);
#1161=LINE('',#5640,#1421);
#1162=LINE('',#5641,#1422);
#1163=LINE('',#5643,#1423);
#1164=LINE('',#5655,#1424);
#1165=LINE('',#5661,#1425);
#1166=LINE('',#5673,#1426);
#1167=LINE('',#5680,#1427);
#1168=LINE('',#5683,#1428);
#1169=LINE('',#5688,#1429);
#1170=LINE('',#5714,#1430);
#1171=LINE('',#5716,#1431);
#1172=LINE('',#5717,#1432);
#1173=LINE('',#5720,#1433);
#1174=LINE('',#5721,#1434);
#1175=LINE('',#5724,#1435);
#1176=LINE('',#5725,#1436);
#1177=LINE('',#5728,#1437);
#1178=LINE('',#5729,#1438);
#1179=LINE('',#5732,#1439);
#1180=LINE('',#5733,#1440);
#1181=LINE('',#5735,#1441);
#1182=LINE('',#5743,#1442);
#1183=LINE('',#5749,#1443);
#1184=LINE('',#5765,#1444);
#1185=LINE('',#5786,#1445);
#1186=LINE('',#5811,#1446);
#1187=LINE('',#5812,#1447);
#1188=LINE('',#5814,#1448);
#1189=LINE('',#5816,#1449);
#1190=LINE('',#5821,#1450);
#1191=LINE('',#5824,#1451);
#1192=LINE('',#5826,#1452);
#1193=VECTOR('',#3824,0.275);
#1194=VECTOR('',#3831,0.275);
#1195=VECTOR('',#3838,0.41);
#1196=VECTOR('',#3845,0.41);
#1197=VECTOR('',#3850,1.);
#1198=VECTOR('',#3853,1.);
#1199=VECTOR('',#3858,1.);
#1200=VECTOR('',#3859,1.);
#1201=VECTOR('',#3860,1.);
#1202=VECTOR('',#3861,1.);
#1203=VECTOR('',#3862,1.);
#1204=VECTOR('',#3865,1.);
#1205=VECTOR('',#3866,1.);
#1206=VECTOR('',#3869,1.);
#1207=VECTOR('',#3870,1.);
#1208=VECTOR('',#3871,1.);
#1209=VECTOR('',#3872,1.);
#1210=VECTOR('',#3875,1.);
#1211=VECTOR('',#3878,1.);
#1212=VECTOR('',#3881,1.);
#1213=VECTOR('',#3882,1.);
#1214=VECTOR('',#3883,1.);
#1215=VECTOR('',#3884,1.);
#1216=VECTOR('',#3885,1.);
#1217=VECTOR('',#3886,1.);
#1218=VECTOR('',#3887,1.);
#1219=VECTOR('',#3888,1.);
#1220=VECTOR('',#3889,1.);
#1221=VECTOR('',#3892,1.);
#1222=VECTOR('',#3895,1.);
#1223=VECTOR('',#3900,1.);
#1224=VECTOR('',#3901,1.);
#1225=VECTOR('',#3902,1.);
#1226=VECTOR('',#3903,1.);
#1227=VECTOR('',#3906,1.);
#1228=VECTOR('',#3907,1.);
#1229=VECTOR('',#3910,1.);
#1230=VECTOR('',#3911,1.);
#1231=VECTOR('',#3912,1.);
#1232=VECTOR('',#3915,1.);
#1233=VECTOR('',#3920,1.);
#1234=VECTOR('',#3921,1.);
#1235=VECTOR('',#3922,1.);
#1236=VECTOR('',#3925,1.);
#1237=VECTOR('',#3926,1.);
#1238=VECTOR('',#3929,1.);
#1239=VECTOR('',#3930,1.);
#1240=VECTOR('',#3933,1.);
#1241=VECTOR('',#3944,0.410000000000047);
#1242=VECTOR('',#3957,0.410000000000047);
#1243=VECTOR('',#3968,0.410000000000047);
#1244=VECTOR('',#3977,0.410000000000047);
#1245=VECTOR('',#3986,1.00000000000011);
#1246=VECTOR('',#3989,1.00000000000011);
#1247=VECTOR('',#3992,1.00000000000011);
#1248=VECTOR('',#3995,1.00000000000011);
#1249=VECTOR('',#3998,1.00000000000011);
#1250=VECTOR('',#3999,1.00000000000011);
#1251=VECTOR('',#4000,1.00000000000011);
#1252=VECTOR('',#4001,1.00000000000011);
#1253=VECTOR('',#4004,1.00000000000011);
#1254=VECTOR('',#4005,1.00000000000011);
#1255=VECTOR('',#4008,1.00000000000011);
#1256=VECTOR('',#4009,1.00000000000011);
#1257=VECTOR('',#4012,1.00000000000011);
#1258=VECTOR('',#4013,1.00000000000011);
#1259=VECTOR('',#4014,1.00000000000011);
#1260=VECTOR('',#4015,1.00000000000011);
#1261=VECTOR('',#4018,1.00000000000011);
#1262=VECTOR('',#4019,1.00000000000011);
#1263=VECTOR('',#4020,1.00000000000011);
#1264=VECTOR('',#4021,1.00000000000011);
#1265=VECTOR('',#4024,1.00000000000011);
#1266=VECTOR('',#4025,1.00000000000011);
#1267=VECTOR('',#4026,1.00000000000011);
#1268=VECTOR('',#4027,1.00000000000011);
#1269=VECTOR('',#4030,1.00000000000011);
#1270=VECTOR('',#4031,1.00000000000011);
#1271=VECTOR('',#4040,1.00000000000011);
#1272=VECTOR('',#4043,1.00000000000011);
#1273=VECTOR('',#4052,1.00000000000011);
#1274=VECTOR('',#4053,1.00000000000011);
#1275=VECTOR('',#4054,1.00000000000011);
#1276=VECTOR('',#4055,1.00000000000011);
#1277=VECTOR('',#4056,1.00000000000011);
#1278=VECTOR('',#4059,1.00000000000011);
#1279=VECTOR('',#4062,1.00000000000011);
#1280=VECTOR('',#4063,1.00000000000011);
#1281=VECTOR('',#4066,1.00000000000011);
#1282=VECTOR('',#4079,1.00000000000011);
#1283=VECTOR('',#4082,1.00000000000011);
#1284=VECTOR('',#4083,1.00000000000011);
#1285=VECTOR('',#4084,1.00000000000011);
#1286=VECTOR('',#4085,1.00000000000011);
#1287=VECTOR('',#4096,1.00000000000011);
#1288=VECTOR('',#4097,1.00000000000011);
#1289=VECTOR('',#4104,1.00000000000011);
#1290=VECTOR('',#4107,1.00000000000011);
#1291=VECTOR('',#4108,1.00000000000011);
#1292=VECTOR('',#4111,1.00000000000011);
#1293=VECTOR('',#4130,0.310000000000035);
#1294=VECTOR('',#4137,0.400000000000046);
#1295=VECTOR('',#4154,0.300000000000034);
#1296=VECTOR('',#4163,0.300000000000034);
#1297=VECTOR('',#4168,0.270000000000031);
#1298=VECTOR('',#4173,0.576175134594879);
#1299=VECTOR('',#4176,1.00000000000011);
#1300=VECTOR('',#4177,1.00000000000011);
#1301=VECTOR('',#4178,1.00000000000011);
#1302=VECTOR('',#4181,1.00000000000011);
#1303=VECTOR('',#4182,1.00000000000011);
#1304=VECTOR('',#4185,1.00000000000011);
#1305=VECTOR('',#4186,1.00000000000011);
#1306=VECTOR('',#4189,1.00000000000011);
#1307=VECTOR('',#4190,1.00000000000011);
#1308=VECTOR('',#4193,1.00000000000011);
#1309=VECTOR('',#4194,1.00000000000011);
#1310=VECTOR('',#4197,1.00000000000011);
#1311=VECTOR('',#4208,0.320000000000037);
#1312=VECTOR('',#4215,0.600000000000068);
#1313=VECTOR('',#4228,0.320000000000037);
#1314=VECTOR('',#4235,0.600000000000068);
#1315=VECTOR('',#4246,0.576175134594879);
#1316=VECTOR('',#4253,0.576175134594879);
#1317=VECTOR('',#4256,1.00000000000011);
#1318=VECTOR('',#4257,1.00000000000011);
#1319=VECTOR('',#4260,1.00000000000011);
#1320=VECTOR('',#4263,1.00000000000011);
#1321=VECTOR('',#4268,0.300000000000034);
#1322=VECTOR('',#4273,1.00000000000011);
#1323=VECTOR('',#4276,1.00000000000011);
#1324=VECTOR('',#4313,0.274999999999999);
#1325=VECTOR('',#4320,0.274999999999999);
#1326=VECTOR('',#4327,0.41);
#1327=VECTOR('',#4334,0.41);
#1328=VECTOR('',#4339,1.);
#1329=VECTOR('',#4342,1.);
#1330=VECTOR('',#4347,1.);
#1331=VECTOR('',#4348,1.);
#1332=VECTOR('',#4349,1.);
#1333=VECTOR('',#4350,1.);
#1334=VECTOR('',#4351,1.);
#1335=VECTOR('',#4354,1.);
#1336=VECTOR('',#4355,1.);
#1337=VECTOR('',#4358,1.);
#1338=VECTOR('',#4359,1.);
#1339=VECTOR('',#4360,1.);
#1340=VECTOR('',#4361,1.);
#1341=VECTOR('',#4364,1.);
#1342=VECTOR('',#4367,1.);
#1343=VECTOR('',#4370,1.);
#1344=VECTOR('',#4371,1.);
#1345=VECTOR('',#4372,1.);
#1346=VECTOR('',#4373,1.);
#1347=VECTOR('',#4374,1.);
#1348=VECTOR('',#4375,1.);
#1349=VECTOR('',#4376,1.);
#1350=VECTOR('',#4377,1.);
#1351=VECTOR('',#4378,1.);
#1352=VECTOR('',#4381,1.);
#1353=VECTOR('',#4384,1.);
#1354=VECTOR('',#4389,1.);
#1355=VECTOR('',#4390,1.);
#1356=VECTOR('',#4391,1.);
#1357=VECTOR('',#4392,1.);
#1358=VECTOR('',#4395,1.);
#1359=VECTOR('',#4396,1.);
#1360=VECTOR('',#4399,1.);
#1361=VECTOR('',#4400,1.);
#1362=VECTOR('',#4401,1.);
#1363=VECTOR('',#4404,1.);
#1364=VECTOR('',#4409,1.);
#1365=VECTOR('',#4410,1.);
#1366=VECTOR('',#4411,1.);
#1367=VECTOR('',#4414,1.);
#1368=VECTOR('',#4415,1.);
#1369=VECTOR('',#4416,1.);
#1370=VECTOR('',#4419,1.);
#1371=VECTOR('',#4420,1.);
#1372=VECTOR('',#4435,0.41);
#1373=VECTOR('',#4448,0.41);
#1374=VECTOR('',#4459,0.41);
#1375=VECTOR('',#4468,0.41);
#1376=VECTOR('',#4477,1.);
#1377=VECTOR('',#4480,1.);
#1378=VECTOR('',#4483,1.);
#1379=VECTOR('',#4486,1.);
#1380=VECTOR('',#4489,1.);
#1381=VECTOR('',#4490,1.);
#1382=VECTOR('',#4491,1.);
#1383=VECTOR('',#4492,1.);
#1384=VECTOR('',#4495,1.);
#1385=VECTOR('',#4496,1.);
#1386=VECTOR('',#4499,1.);
#1387=VECTOR('',#4500,1.);
#1388=VECTOR('',#4503,1.);
#1389=VECTOR('',#4504,1.);
#1390=VECTOR('',#4505,1.);
#1391=VECTOR('',#4506,1.);
#1392=VECTOR('',#4509,1.);
#1393=VECTOR('',#4510,1.);
#1394=VECTOR('',#4511,1.);
#1395=VECTOR('',#4512,1.);
#1396=VECTOR('',#4515,1.);
#1397=VECTOR('',#4516,1.);
#1398=VECTOR('',#4517,1.);
#1399=VECTOR('',#4518,1.);
#1400=VECTOR('',#4521,1.);
#1401=VECTOR('',#4522,1.);
#1402=VECTOR('',#4531,1.);
#1403=VECTOR('',#4534,1.);
#1404=VECTOR('',#4543,1.);
#1405=VECTOR('',#4544,1.);
#1406=VECTOR('',#4545,1.);
#1407=VECTOR('',#4546,1.);
#1408=VECTOR('',#4547,1.);
#1409=VECTOR('',#4550,1.);
#1410=VECTOR('',#4553,1.);
#1411=VECTOR('',#4554,1.);
#1412=VECTOR('',#4557,1.);
#1413=VECTOR('',#4570,1.);
#1414=VECTOR('',#4573,1.);
#1415=VECTOR('',#4574,1.);
#1416=VECTOR('',#4575,1.);
#1417=VECTOR('',#4576,1.);
#1418=VECTOR('',#4587,1.);
#1419=VECTOR('',#4588,1.);
#1420=VECTOR('',#4595,1.);
#1421=VECTOR('',#4598,1.);
#1422=VECTOR('',#4599,1.);
#1423=VECTOR('',#4602,1.);
#1424=VECTOR('',#4621,0.31);
#1425=VECTOR('',#4628,0.4);
#1426=VECTOR('',#4645,0.3);
#1427=VECTOR('',#4654,0.3);
#1428=VECTOR('',#4659,0.27);
#1429=VECTOR('',#4664,0.576175134594813);
#1430=VECTOR('',#4667,1.);
#1431=VECTOR('',#4668,1.);
#1432=VECTOR('',#4669,1.);
#1433=VECTOR('',#4672,1.);
#1434=VECTOR('',#4673,1.);
#1435=VECTOR('',#4676,1.);
#1436=VECTOR('',#4677,1.);
#1437=VECTOR('',#4680,1.);
#1438=VECTOR('',#4681,1.);
#1439=VECTOR('',#4684,1.);
#1440=VECTOR('',#4685,1.);
#1441=VECTOR('',#4688,1.);
#1442=VECTOR('',#4699,0.32);
#1443=VECTOR('',#4706,0.6);
#1444=VECTOR('',#4717,0.576175134594813);
#1445=VECTOR('',#4724,0.576175134594813);
#1446=VECTOR('',#4727,1.);
#1447=VECTOR('',#4728,1.);
#1448=VECTOR('',#4731,1.);
#1449=VECTOR('',#4734,1.);
#1450=VECTOR('',#4739,0.3);
#1451=VECTOR('',#4744,1.);
#1452=VECTOR('',#4747,1.);
#1453=CIRCLE('',#3426,0.275);
#1454=CIRCLE('',#3427,0.275);
#1455=CIRCLE('',#3429,0.275);
#1456=CIRCLE('',#3430,0.275);
#1457=CIRCLE('',#3432,0.41);
#1458=CIRCLE('',#3433,0.41);
#1459=CIRCLE('',#3435,0.41);
#1460=CIRCLE('',#3436,0.41);
#1461=CIRCLE('',#3438,0.7);
#1462=CIRCLE('',#3439,0.7);
#1463=CIRCLE('',#3447,0.7);
#1464=CIRCLE('',#3448,0.7);
#1465=CIRCLE('',#3462,0.410000000000047);
#1466=CIRCLE('',#3463,0.410000000000047);
#1467=CIRCLE('',#3465,0.410000000000047);
#1468=CIRCLE('',#3468,0.410000000000047);
#1469=CIRCLE('',#3469,0.410000000000047);
#1470=CIRCLE('',#3470,0.410000000000047);
#1471=CIRCLE('',#3472,0.410000000000047);
#1472=CIRCLE('',#3474,0.410000000000047);
#1473=CIRCLE('',#3477,0.410000000000047);
#1474=CIRCLE('',#3479,0.410000000000047);
#1475=CIRCLE('',#3482,0.70000000000008);
#1476=CIRCLE('',#3484,0.70000000000008);
#1477=CIRCLE('',#3493,0.70000000000008);
#1478=CIRCLE('',#3494,0.70000000000008);
#1479=CIRCLE('',#3496,0.70000000000008);
#1480=CIRCLE('',#3505,0.70000000000008);
#1481=CIRCLE('',#3507,0.70000000000008);
#1482=CIRCLE('',#3512,0.70000000000008);
#1483=CIRCLE('',#3513,0.70000000000008);
#1484=CIRCLE('',#3516,0.70000000000008);
#1485=CIRCLE('',#3523,0.70000000000008);
#1486=CIRCLE('',#3524,0.70000000000008);
#1487=CIRCLE('',#3529,0.310000000000035);
#1488=CIRCLE('',#3530,0.310000000000035);
#1489=CIRCLE('',#3532,0.400000000000046);
#1490=CIRCLE('',#3533,0.400000000000046);
#1491=CIRCLE('',#3538,0.300000000000034);
#1492=CIRCLE('',#3539,0.250000000000028);
#1493=CIRCLE('',#3541,0.300000000000034);
#1494=CIRCLE('',#3544,0.294200000000034);
#1495=CIRCLE('',#3545,0.294200000000034);
#1496=CIRCLE('',#3548,0.475000000000054);
#1497=CIRCLE('',#3559,0.320000000000037);
#1498=CIRCLE('',#3560,0.320000000000037);
#1499=CIRCLE('',#3562,0.600000000000069);
#1500=CIRCLE('',#3563,0.600000000000069);
#1501=CIRCLE('',#3568,0.320000000000037);
#1502=CIRCLE('',#3569,0.320000000000037);
#1503=CIRCLE('',#3571,0.600000000000069);
#1504=CIRCLE('',#3572,0.600000000000069);
#1505=CIRCLE('',#3577,0.475000000000054);
#1506=CIRCLE('',#3579,0.475000000000054);
#1507=CIRCLE('',#3584,0.251750000000029);
#1508=CIRCLE('',#3585,0.251750000000029);
#1509=CIRCLE('',#3605,0.274999999999999);
#1510=CIRCLE('',#3606,0.274999999999999);
#1511=CIRCLE('',#3608,0.274999999999999);
#1512=CIRCLE('',#3609,0.274999999999999);
#1513=CIRCLE('',#3611,0.41);
#1514=CIRCLE('',#3612,0.41);
#1515=CIRCLE('',#3614,0.41);
#1516=CIRCLE('',#3615,0.41);
#1517=CIRCLE('',#3617,0.699999999999999);
#1518=CIRCLE('',#3618,0.699999999999999);
#1519=CIRCLE('',#3626,0.699999999999999);
#1520=CIRCLE('',#3627,0.699999999999999);
#1521=CIRCLE('',#3642,0.41);
#1522=CIRCLE('',#3643,0.41);
#1523=CIRCLE('',#3645,0.41);
#1524=CIRCLE('',#3648,0.41);
#1525=CIRCLE('',#3649,0.41);
#1526=CIRCLE('',#3650,0.41);
#1527=CIRCLE('',#3652,0.41);
#1528=CIRCLE('',#3654,0.41);
#1529=CIRCLE('',#3657,0.41);
#1530=CIRCLE('',#3659,0.41);
#1531=CIRCLE('',#3662,0.7);
#1532=CIRCLE('',#3664,0.7);
#1533=CIRCLE('',#3673,0.7);
#1534=CIRCLE('',#3674,0.7);
#1535=CIRCLE('',#3676,0.7);
#1536=CIRCLE('',#3685,0.7);
#1537=CIRCLE('',#3687,0.7);
#1538=CIRCLE('',#3692,0.7);
#1539=CIRCLE('',#3693,0.7);
#1540=CIRCLE('',#3696,0.7);
#1541=CIRCLE('',#3703,0.7);
#1542=CIRCLE('',#3704,0.7);
#1543=CIRCLE('',#3709,0.31);
#1544=CIRCLE('',#3710,0.31);
#1545=CIRCLE('',#3712,0.4);
#1546=CIRCLE('',#3713,0.4);
#1547=CIRCLE('',#3718,0.3);
#1548=CIRCLE('',#3719,0.25);
#1549=CIRCLE('',#3721,0.3);
#1550=CIRCLE('',#3724,0.2942);
#1551=CIRCLE('',#3725,0.2942);
#1552=CIRCLE('',#3728,0.475);
#1553=CIRCLE('',#3739,0.32);
#1554=CIRCLE('',#3740,0.32);
#1555=CIRCLE('',#3742,0.6);
#1556=CIRCLE('',#3743,0.6);
#1557=CIRCLE('',#3748,0.475);
#1558=CIRCLE('',#3750,0.475);
#1559=CIRCLE('',#3755,0.25175);
#1560=CIRCLE('',#3756,0.25175);
#1561=VERTEX_POINT('',#4862);
#1562=VERTEX_POINT('',#4864);
#1563=VERTEX_POINT('',#4868);
#1564=VERTEX_POINT('',#4870);
#1565=VERTEX_POINT('',#4874);
#1566=VERTEX_POINT('',#4876);
#1567=VERTEX_POINT('',#4880);
#1568=VERTEX_POINT('',#4882);
#1569=VERTEX_POINT('',#4886);
#1570=VERTEX_POINT('',#4887);
#1571=VERTEX_POINT('',#4889);
#1572=VERTEX_POINT('',#4891);
#1573=VERTEX_POINT('',#4895);
#1574=VERTEX_POINT('',#4897);
#1575=VERTEX_POINT('',#4899);
#1576=VERTEX_POINT('',#4901);
#1577=VERTEX_POINT('',#4905);
#1578=VERTEX_POINT('',#4909);
#1579=VERTEX_POINT('',#4911);
#1580=VERTEX_POINT('',#4913);
#1581=VERTEX_POINT('',#4921);
#1582=VERTEX_POINT('',#4923);
#1583=VERTEX_POINT('',#4925);
#1584=VERTEX_POINT('',#4927);
#1585=VERTEX_POINT('',#4929);
#1586=VERTEX_POINT('',#4931);
#1587=VERTEX_POINT('',#4933);
#1588=VERTEX_POINT('',#4935);
#1589=VERTEX_POINT('',#4939);
#1590=VERTEX_POINT('',#4940);
#1591=VERTEX_POINT('',#4942);
#1592=VERTEX_POINT('',#4944);
#1593=VERTEX_POINT('',#4948);
#1594=VERTEX_POINT('',#4950);
#1595=VERTEX_POINT('',#4955);
#1596=VERTEX_POINT('',#4960);
#1597=VERTEX_POINT('',#4967);
#1598=VERTEX_POINT('',#4968);
#1599=VERTEX_POINT('',#4973);
#1600=VERTEX_POINT('',#4977);
#1601=VERTEX_POINT('',#4986);
#1602=VERTEX_POINT('',#4988);
#1603=VERTEX_POINT('',#4990);
#1604=VERTEX_POINT('',#4992);
#1605=VERTEX_POINT('',#4996);
#1606=VERTEX_POINT('',#4997);
#1607=VERTEX_POINT('',#4999);
#1608=VERTEX_POINT('',#5001);
#1609=VERTEX_POINT('',#5006);
#1610=VERTEX_POINT('',#5007);
#1611=VERTEX_POINT('',#5009);
#1612=VERTEX_POINT('',#5011);
#1613=VERTEX_POINT('',#5016);
#1614=VERTEX_POINT('',#5018);
#1615=VERTEX_POINT('',#5020);
#1616=VERTEX_POINT('',#5022);
#1617=VERTEX_POINT('',#5026);
#1618=VERTEX_POINT('',#5028);
#1619=VERTEX_POINT('',#5032);
#1620=VERTEX_POINT('',#5034);
#1621=VERTEX_POINT('',#5038);
#1622=VERTEX_POINT('',#5040);
#1623=VERTEX_POINT('',#5042);
#1624=VERTEX_POINT('',#5044);
#1625=VERTEX_POINT('',#5046);
#1626=VERTEX_POINT('',#5048);
#1627=VERTEX_POINT('',#5052);
#1628=VERTEX_POINT('',#5054);
#1629=VERTEX_POINT('',#5056);
#1630=VERTEX_POINT('',#5058);
#1631=VERTEX_POINT('',#5060);
#1632=VERTEX_POINT('',#5062);
#1633=VERTEX_POINT('',#5066);
#1634=VERTEX_POINT('',#5067);
#1635=VERTEX_POINT('',#5069);
#1636=VERTEX_POINT('',#5071);
#1637=VERTEX_POINT('',#5075);
#1638=VERTEX_POINT('',#5076);
#1639=VERTEX_POINT('',#5078);
#1640=VERTEX_POINT('',#5080);
#1641=VERTEX_POINT('',#5087);
#1642=VERTEX_POINT('',#5088);
#1643=VERTEX_POINT('',#5099);
#1644=VERTEX_POINT('',#5102);
#1645=VERTEX_POINT('',#5119);
#1646=VERTEX_POINT('',#5121);
#1647=VERTEX_POINT('',#5123);
#1648=VERTEX_POINT('',#5126);
#1649=VERTEX_POINT('',#5153);
#1650=VERTEX_POINT('',#5155);
#1651=VERTEX_POINT('',#5159);
#1652=VERTEX_POINT('',#5161);
#1653=VERTEX_POINT('',#5168);
#1654=VERTEX_POINT('',#5170);
#1655=VERTEX_POINT('',#5173);
#1656=VERTEX_POINT('',#5178);
#1657=VERTEX_POINT('',#5180);
#1658=VERTEX_POINT('',#5186);
#1659=VERTEX_POINT('',#5188);
#1660=VERTEX_POINT('',#5190);
#1661=VERTEX_POINT('',#5194);
#1662=VERTEX_POINT('',#5198);
#1663=VERTEX_POINT('',#5202);
#1664=VERTEX_POINT('',#5206);
#1665=VERTEX_POINT('',#5214);
#1666=VERTEX_POINT('',#5216);
#1667=VERTEX_POINT('',#5220);
#1668=VERTEX_POINT('',#5224);
#1669=VERTEX_POINT('',#5228);
#1670=VERTEX_POINT('',#5232);
#1671=VERTEX_POINT('',#5241);
#1672=VERTEX_POINT('',#5243);
#1673=VERTEX_POINT('',#5247);
#1674=VERTEX_POINT('',#5249);
#1675=VERTEX_POINT('',#5256);
#1676=VERTEX_POINT('',#5258);
#1677=VERTEX_POINT('',#5262);
#1678=VERTEX_POINT('',#5264);
#1679=VERTEX_POINT('',#5271);
#1680=VERTEX_POINT('',#5272);
#1681=VERTEX_POINT('',#5276);
#1682=VERTEX_POINT('',#5280);
#1683=VERTEX_POINT('',#5283);
#1684=VERTEX_POINT('',#5287);
#1685=VERTEX_POINT('',#5291);
#1686=VERTEX_POINT('',#5299);
#1687=VERTEX_POINT('',#5301);
#1688=VERTEX_POINT('',#5303);
#1689=VERTEX_POINT('',#5307);
#1690=VERTEX_POINT('',#5311);
#1691=VERTEX_POINT('',#5315);
#1692=VERTEX_POINT('',#5319);
#1693=VERTEX_POINT('',#5334);
#1694=VERTEX_POINT('',#5336);
#1695=VERTEX_POINT('',#5360);
#1696=VERTEX_POINT('',#5362);
#1697=VERTEX_POINT('',#5366);
#1698=VERTEX_POINT('',#5368);
#1699=VERTEX_POINT('',#5372);
#1700=VERTEX_POINT('',#5374);
#1701=VERTEX_POINT('',#5378);
#1702=VERTEX_POINT('',#5380);
#1703=VERTEX_POINT('',#5384);
#1704=VERTEX_POINT('',#5385);
#1705=VERTEX_POINT('',#5387);
#1706=VERTEX_POINT('',#5389);
#1707=VERTEX_POINT('',#5393);
#1708=VERTEX_POINT('',#5395);
#1709=VERTEX_POINT('',#5397);
#1710=VERTEX_POINT('',#5399);
#1711=VERTEX_POINT('',#5403);
#1712=VERTEX_POINT('',#5407);
#1713=VERTEX_POINT('',#5409);
#1714=VERTEX_POINT('',#5411);
#1715=VERTEX_POINT('',#5419);
#1716=VERTEX_POINT('',#5421);
#1717=VERTEX_POINT('',#5423);
#1718=VERTEX_POINT('',#5425);
#1719=VERTEX_POINT('',#5427);
#1720=VERTEX_POINT('',#5429);
#1721=VERTEX_POINT('',#5431);
#1722=VERTEX_POINT('',#5433);
#1723=VERTEX_POINT('',#5437);
#1724=VERTEX_POINT('',#5438);
#1725=VERTEX_POINT('',#5440);
#1726=VERTEX_POINT('',#5442);
#1727=VERTEX_POINT('',#5446);
#1728=VERTEX_POINT('',#5449);
#1729=VERTEX_POINT('',#5453);
#1730=VERTEX_POINT('',#5457);
#1731=VERTEX_POINT('',#5465);
#1732=VERTEX_POINT('',#5467);
#1733=VERTEX_POINT('',#5471);
#1734=VERTEX_POINT('',#5473);
#1735=VERTEX_POINT('',#5485);
#1736=VERTEX_POINT('',#5487);
#1737=VERTEX_POINT('',#5489);
#1738=VERTEX_POINT('',#5491);
#1739=VERTEX_POINT('',#5495);
#1740=VERTEX_POINT('',#5496);
#1741=VERTEX_POINT('',#5498);
#1742=VERTEX_POINT('',#5500);
#1743=VERTEX_POINT('',#5505);
#1744=VERTEX_POINT('',#5506);
#1745=VERTEX_POINT('',#5508);
#1746=VERTEX_POINT('',#5510);
#1747=VERTEX_POINT('',#5515);
#1748=VERTEX_POINT('',#5517);
#1749=VERTEX_POINT('',#5519);
#1750=VERTEX_POINT('',#5521);
#1751=VERTEX_POINT('',#5525);
#1752=VERTEX_POINT('',#5527);
#1753=VERTEX_POINT('',#5531);
#1754=VERTEX_POINT('',#5533);
#1755=VERTEX_POINT('',#5537);
#1756=VERTEX_POINT('',#5539);
#1757=VERTEX_POINT('',#5541);
#1758=VERTEX_POINT('',#5543);
#1759=VERTEX_POINT('',#5545);
#1760=VERTEX_POINT('',#5547);
#1761=VERTEX_POINT('',#5551);
#1762=VERTEX_POINT('',#5553);
#1763=VERTEX_POINT('',#5555);
#1764=VERTEX_POINT('',#5557);
#1765=VERTEX_POINT('',#5559);
#1766=VERTEX_POINT('',#5561);
#1767=VERTEX_POINT('',#5565);
#1768=VERTEX_POINT('',#5566);
#1769=VERTEX_POINT('',#5568);
#1770=VERTEX_POINT('',#5570);
#1771=VERTEX_POINT('',#5574);
#1772=VERTEX_POINT('',#5575);
#1773=VERTEX_POINT('',#5577);
#1774=VERTEX_POINT('',#5579);
#1775=VERTEX_POINT('',#5586);
#1776=VERTEX_POINT('',#5587);
#1777=VERTEX_POINT('',#5598);
#1778=VERTEX_POINT('',#5601);
#1779=VERTEX_POINT('',#5618);
#1780=VERTEX_POINT('',#5620);
#1781=VERTEX_POINT('',#5622);
#1782=VERTEX_POINT('',#5625);
#1783=VERTEX_POINT('',#5652);
#1784=VERTEX_POINT('',#5654);
#1785=VERTEX_POINT('',#5658);
#1786=VERTEX_POINT('',#5660);
#1787=VERTEX_POINT('',#5667);
#1788=VERTEX_POINT('',#5669);
#1789=VERTEX_POINT('',#5672);
#1790=VERTEX_POINT('',#5677);
#1791=VERTEX_POINT('',#5679);
#1792=VERTEX_POINT('',#5685);
#1793=VERTEX_POINT('',#5687);
#1794=VERTEX_POINT('',#5689);
#1795=VERTEX_POINT('',#5693);
#1796=VERTEX_POINT('',#5697);
#1797=VERTEX_POINT('',#5701);
#1798=VERTEX_POINT('',#5705);
#1799=VERTEX_POINT('',#5713);
#1800=VERTEX_POINT('',#5715);
#1801=VERTEX_POINT('',#5719);
#1802=VERTEX_POINT('',#5723);
#1803=VERTEX_POINT('',#5727);
#1804=VERTEX_POINT('',#5731);
#1805=VERTEX_POINT('',#5740);
#1806=VERTEX_POINT('',#5742);
#1807=VERTEX_POINT('',#5746);
#1808=VERTEX_POINT('',#5748);
#1809=VERTEX_POINT('',#5755);
#1810=VERTEX_POINT('',#5756);
#1811=VERTEX_POINT('',#5760);
#1812=VERTEX_POINT('',#5764);
#1813=VERTEX_POINT('',#5767);
#1814=VERTEX_POINT('',#5771);
#1815=VERTEX_POINT('',#5775);
#1816=VERTEX_POINT('',#5783);
#1817=VERTEX_POINT('',#5785);
#1818=VERTEX_POINT('',#5787);
#1819=VERTEX_POINT('',#5791);
#1820=VERTEX_POINT('',#5795);
#1821=VERTEX_POINT('',#5799);
#1822=VERTEX_POINT('',#5803);
#1823=VERTEX_POINT('',#5818);
#1824=VERTEX_POINT('',#5820);
#1825=EDGE_CURVE('',#1561,#1561,#1453,.T.);
#1826=EDGE_CURVE('',#1561,#1562,#933,.T.);
#1827=EDGE_CURVE('',#1562,#1562,#1454,.T.);
#1828=EDGE_CURVE('',#1563,#1563,#1455,.T.);
#1829=EDGE_CURVE('',#1563,#1564,#934,.T.);
#1830=EDGE_CURVE('',#1564,#1564,#1456,.T.);
#1831=EDGE_CURVE('',#1565,#1565,#1457,.T.);
#1832=EDGE_CURVE('',#1565,#1566,#935,.T.);
#1833=EDGE_CURVE('',#1566,#1566,#1458,.T.);
#1834=EDGE_CURVE('',#1567,#1567,#1459,.T.);
#1835=EDGE_CURVE('',#1567,#1568,#936,.T.);
#1836=EDGE_CURVE('',#1568,#1568,#1460,.T.);
#1837=EDGE_CURVE('',#1569,#1570,#937,.T.);
#1838=EDGE_CURVE('',#1569,#1571,#1461,.T.);
#1839=EDGE_CURVE('',#1572,#1571,#938,.T.);
#1840=EDGE_CURVE('',#1570,#1572,#1462,.T.);
#1841=EDGE_CURVE('',#1572,#1573,#939,.T.);
#1842=EDGE_CURVE('',#1573,#1574,#940,.T.);
#1843=EDGE_CURVE('',#1575,#1574,#941,.T.);
#1844=EDGE_CURVE('',#1576,#1575,#942,.T.);
#1845=EDGE_CURVE('',#1576,#1570,#943,.T.);
#1846=EDGE_CURVE('',#1577,#1571,#944,.T.);
#1847=EDGE_CURVE('',#1577,#1573,#945,.T.);
#1848=EDGE_CURVE('',#1569,#1578,#946,.T.);
#1849=EDGE_CURVE('',#1579,#1578,#947,.T.);
#1850=EDGE_CURVE('',#1580,#1579,#948,.T.);
#1851=EDGE_CURVE('',#1580,#1577,#949,.T.);
#1852=EDGE_CURVE('',#1574,#1580,#950,.T.);
#1853=EDGE_CURVE('',#1578,#1576,#951,.T.);
#1854=EDGE_CURVE('',#1575,#1581,#952,.T.);
#1855=EDGE_CURVE('',#1581,#1582,#953,.T.);
#1856=EDGE_CURVE('',#1582,#1583,#954,.T.);
#1857=EDGE_CURVE('',#1583,#1584,#955,.T.);
#1858=EDGE_CURVE('',#1584,#1585,#956,.T.);
#1859=EDGE_CURVE('',#1585,#1586,#957,.T.);
#1860=EDGE_CURVE('',#1586,#1587,#958,.T.);
#1861=EDGE_CURVE('',#1587,#1588,#959,.T.);
#1862=EDGE_CURVE('',#1588,#1579,#960,.T.);
#1863=EDGE_CURVE('',#1589,#1590,#961,.T.);
#1864=EDGE_CURVE('',#1589,#1591,#1463,.T.);
#1865=EDGE_CURVE('',#1592,#1591,#962,.T.);
#1866=EDGE_CURVE('',#1590,#1592,#1464,.T.);
#1867=EDGE_CURVE('',#1592,#1593,#963,.T.);
#1868=EDGE_CURVE('',#1593,#1594,#964,.T.);
#1869=EDGE_CURVE('',#1588,#1594,#965,.T.);
#1870=EDGE_CURVE('',#1587,#1590,#966,.T.);
#1871=EDGE_CURVE('',#1595,#1591,#967,.T.);
#1872=EDGE_CURVE('',#1595,#1593,#968,.T.);
#1873=EDGE_CURVE('',#1589,#1586,#969,.T.);
#1874=EDGE_CURVE('',#1596,#1585,#970,.T.);
#1875=EDGE_CURVE('',#1596,#1595,#971,.T.);
#1876=EDGE_CURVE('',#1594,#1596,#972,.T.);
#1877=EDGE_CURVE('',#1597,#1598,#973,.T.);
#1878=EDGE_CURVE('',#1598,#1582,#974,.T.);
#1879=EDGE_CURVE('',#1597,#1581,#975,.T.);
#1880=EDGE_CURVE('',#1599,#1584,#976,.T.);
#1881=EDGE_CURVE('',#1599,#1597,#977,.T.);
#1882=EDGE_CURVE('',#1600,#1599,#978,.T.);
#1883=EDGE_CURVE('',#1600,#1583,#979,.T.);
#1884=EDGE_CURVE('',#1598,#1600,#980,.T.);
#1885=EDGE_CURVE('',#1601,#1601,#1465,.T.);
#1886=EDGE_CURVE('',#1601,#1602,#981,.T.);
#1887=EDGE_CURVE('',#1603,#1602,#1466,.T.);
#1888=EDGE_CURVE('',#1604,#1603,#291,.T.);
#1889=EDGE_CURVE('',#1602,#1604,#1467,.T.);
#1890=EDGE_CURVE('',#1605,#1606,#292,.T.);
#1891=EDGE_CURVE('',#1607,#1605,#1468,.T.);
#1892=EDGE_CURVE('',#1607,#1608,#982,.T.);
#1893=EDGE_CURVE('',#1608,#1608,#1469,.T.);
#1894=EDGE_CURVE('',#1606,#1607,#1470,.T.);
#1895=EDGE_CURVE('',#1609,#1610,#1471,.T.);
#1896=EDGE_CURVE('',#1611,#1609,#293,.T.);
#1897=EDGE_CURVE('',#1611,#1612,#983,.T.);
#1898=EDGE_CURVE('',#1612,#1612,#1472,.T.);
#1899=EDGE_CURVE('',#1610,#1611,#294,.T.);
#1900=EDGE_CURVE('',#1613,#1613,#1473,.T.);
#1901=EDGE_CURVE('',#1613,#1614,#984,.T.);
#1902=EDGE_CURVE('',#1615,#1614,#295,.T.);
#1903=EDGE_CURVE('',#1616,#1615,#1474,.T.);
#1904=EDGE_CURVE('',#1614,#1616,#296,.T.);
#1905=EDGE_CURVE('',#1605,#1617,#985,.T.);
#1906=EDGE_CURVE('',#1618,#1617,#1475,.T.);
#1907=EDGE_CURVE('',#1618,#1606,#986,.T.);
#1908=EDGE_CURVE('',#1604,#1619,#987,.T.);
#1909=EDGE_CURVE('',#1619,#1620,#1476,.T.);
#1910=EDGE_CURVE('',#1620,#1603,#988,.T.);
#1911=EDGE_CURVE('',#1621,#1616,#989,.T.);
#1912=EDGE_CURVE('',#1622,#1621,#990,.T.);
#1913=EDGE_CURVE('',#1622,#1623,#991,.T.);
#1914=EDGE_CURVE('',#1623,#1624,#992,.T.);
#1915=EDGE_CURVE('',#1625,#1624,#297,.T.);
#1916=EDGE_CURVE('',#1626,#1625,#993,.T.);
#1917=EDGE_CURVE('',#1615,#1626,#994,.T.);
#1918=EDGE_CURVE('',#1609,#1627,#995,.T.);
#1919=EDGE_CURVE('',#1628,#1627,#996,.T.);
#1920=EDGE_CURVE('',#1629,#1628,#298,.T.);
#1921=EDGE_CURVE('',#1630,#1629,#997,.T.);
#1922=EDGE_CURVE('',#1630,#1631,#998,.T.);
#1923=EDGE_CURVE('',#1631,#1632,#999,.T.);
#1924=EDGE_CURVE('',#1632,#1610,#1000,.T.);
#1925=EDGE_CURVE('',#1633,#1634,#1001,.T.);
#1926=EDGE_CURVE('',#1635,#1633,#1002,.T.);
#1927=EDGE_CURVE('',#1636,#1635,#1003,.T.);
#1928=EDGE_CURVE('',#1636,#1634,#1004,.T.);
#1929=EDGE_CURVE('',#1637,#1638,#1005,.T.);
#1930=EDGE_CURVE('',#1637,#1639,#1006,.T.);
#1931=EDGE_CURVE('',#1640,#1639,#1007,.T.);
#1932=EDGE_CURVE('',#1638,#1640,#1008,.T.);
#1933=EDGE_CURVE('',#1638,#1633,#1009,.T.);
#1934=EDGE_CURVE('',#1635,#1640,#1010,.T.);
#1935=EDGE_CURVE('',#1641,#1642,#1477,.T.);
#1936=EDGE_CURVE('',#1642,#1641,#1478,.T.);
#1937=EDGE_CURVE('',#1621,#1641,#1011,.T.);
#1938=EDGE_CURVE('',#1626,#1621,#1479,.T.);
#1939=EDGE_CURVE('',#1642,#1626,#1012,.T.);
#1940=EDGE_CURVE('',#1641,#1642,#299,.T.);
#1941=EDGE_CURVE('',#1643,#1618,#1013,.T.);
#1942=EDGE_CURVE('',#1643,#1636,#1014,.T.);
#1943=EDGE_CURVE('',#1639,#1644,#1015,.T.);
#1944=EDGE_CURVE('',#1644,#1641,#1016,.T.);
#1945=EDGE_CURVE('',#1617,#1642,#1017,.T.);
#1946=EDGE_CURVE('',#1644,#1622,#1018,.T.);
#1947=EDGE_CURVE('',#1624,#1618,#1019,.T.);
#1948=EDGE_CURVE('',#1623,#1643,#1020,.T.);
#1949=EDGE_CURVE('',#1617,#1625,#1021,.T.);
#1950=EDGE_CURVE('',#1625,#1624,#1480,.T.);
#1951=EDGE_CURVE('',#1624,#1625,#1481,.T.);
#1952=EDGE_CURVE('',#1645,#1620,#1022,.T.);
#1953=EDGE_CURVE('',#1645,#1646,#300,.T.);
#1954=EDGE_CURVE('',#1647,#1646,#1023,.T.);
#1955=EDGE_CURVE('',#1647,#1637,#1024,.T.);
#1956=EDGE_CURVE('',#1634,#1648,#1025,.T.);
#1957=EDGE_CURVE('',#1648,#1619,#1026,.T.);
#1958=EDGE_CURVE('',#1645,#1646,#1482,.T.);
#1959=EDGE_CURVE('',#1646,#1645,#1483,.T.);
#1960=EDGE_CURVE('',#1646,#1632,#1027,.T.);
#1961=EDGE_CURVE('',#1627,#1645,#1028,.T.);
#1962=EDGE_CURVE('',#1627,#1632,#1484,.T.);
#1963=EDGE_CURVE('',#1631,#1647,#1029,.T.);
#1964=EDGE_CURVE('',#1619,#1629,#1030,.T.);
#1965=EDGE_CURVE('',#1648,#1630,#1031,.T.);
#1966=EDGE_CURVE('',#1628,#1620,#1032,.T.);
#1967=EDGE_CURVE('',#1628,#1629,#1485,.T.);
#1968=EDGE_CURVE('',#1629,#1628,#1486,.T.);
#1969=EDGE_CURVE('',#1649,#1649,#1487,.T.);
#1970=EDGE_CURVE('',#1649,#1650,#1033,.T.);
#1971=EDGE_CURVE('',#1650,#1650,#1488,.T.);
#1972=EDGE_CURVE('',#1651,#1651,#1489,.T.);
#1973=EDGE_CURVE('',#1651,#1652,#1034,.T.);
#1974=EDGE_CURVE('',#1652,#1652,#1490,.T.);
#1975=EDGE_CURVE('',#1653,#1653,#1491,.T.);
#1976=EDGE_CURVE('',#1654,#1654,#1492,.T.);
#1977=EDGE_CURVE('',#1653,#1655,#1035,.T.);
#1978=EDGE_CURVE('',#1655,#1655,#1493,.T.);
#1979=EDGE_CURVE('',#1656,#1656,#1494,.F.);
#1980=EDGE_CURVE('',#1656,#1657,#1036,.T.);
#1981=EDGE_CURVE('',#1657,#1657,#1495,.F.);
#1982=EDGE_CURVE('',#1654,#1656,#1037,.T.);
#1983=EDGE_CURVE('',#1658,#1658,#1496,.T.);
#1984=EDGE_CURVE('',#1658,#1659,#1038,.T.);
#1985=EDGE_CURVE('',#1660,#1659,#247,.T.);
#1986=EDGE_CURVE('',#1661,#1660,#248,.T.);
#1987=EDGE_CURVE('',#1662,#1661,#249,.T.);
#1988=EDGE_CURVE('',#1663,#1662,#250,.T.);
#1989=EDGE_CURVE('',#1664,#1663,#251,.T.);
#1990=EDGE_CURVE('',#1659,#1664,#252,.T.);
#1991=EDGE_CURVE('',#1665,#1663,#1039,.T.);
#1992=EDGE_CURVE('',#1665,#1666,#1040,.T.);
#1993=EDGE_CURVE('',#1666,#1664,#1041,.T.);
#1994=EDGE_CURVE('',#1667,#1662,#1042,.T.);
#1995=EDGE_CURVE('',#1667,#1665,#1043,.T.);
#1996=EDGE_CURVE('',#1668,#1661,#1044,.T.);
#1997=EDGE_CURVE('',#1668,#1667,#1045,.T.);
#1998=EDGE_CURVE('',#1669,#1660,#1046,.T.);
#1999=EDGE_CURVE('',#1669,#1668,#1047,.T.);
#2000=EDGE_CURVE('',#1670,#1659,#1048,.T.);
#2001=EDGE_CURVE('',#1670,#1669,#1049,.T.);
#2002=EDGE_CURVE('',#1666,#1670,#1050,.T.);
#2003=EDGE_CURVE('',#1671,#1671,#1497,.T.);
#2004=EDGE_CURVE('',#1671,#1672,#1051,.T.);
#2005=EDGE_CURVE('',#1672,#1672,#1498,.T.);
#2006=EDGE_CURVE('',#1673,#1673,#1499,.T.);
#2007=EDGE_CURVE('',#1673,#1674,#1052,.T.);
#2008=EDGE_CURVE('',#1674,#1674,#1500,.T.);
#2009=EDGE_CURVE('',#1675,#1675,#1501,.T.);
#2010=EDGE_CURVE('',#1675,#1676,#1053,.T.);
#2011=EDGE_CURVE('',#1676,#1676,#1502,.T.);
#2012=EDGE_CURVE('',#1677,#1677,#1503,.T.);
#2013=EDGE_CURVE('',#1677,#1678,#1054,.T.);
#2014=EDGE_CURVE('',#1678,#1678,#1504,.T.);
#2015=EDGE_CURVE('',#1679,#1680,#253,.T.);
#2016=EDGE_CURVE('',#1681,#1679,#254,.T.);
#2017=EDGE_CURVE('',#1681,#1682,#1055,.T.);
#2018=EDGE_CURVE('',#1682,#1682,#1505,.T.);
#2019=EDGE_CURVE('',#1683,#1681,#255,.T.);
#2020=EDGE_CURVE('',#1684,#1683,#256,.T.);
#2021=EDGE_CURVE('',#1685,#1684,#257,.T.);
#2022=EDGE_CURVE('',#1680,#1685,#258,.T.);
#2023=EDGE_CURVE('',#1686,#1686,#1506,.T.);
#2024=EDGE_CURVE('',#1686,#1687,#1056,.T.);
#2025=EDGE_CURVE('',#1688,#1687,#259,.T.);
#2026=EDGE_CURVE('',#1689,#1688,#260,.T.);
#2027=EDGE_CURVE('',#1690,#1689,#261,.T.);
#2028=EDGE_CURVE('',#1691,#1690,#262,.T.);
#2029=EDGE_CURVE('',#1692,#1691,#263,.T.);
#2030=EDGE_CURVE('',#1687,#1692,#264,.T.);
#2031=EDGE_CURVE('',#1683,#1692,#1057,.T.);
#2032=EDGE_CURVE('',#1684,#1691,#1058,.T.);
#2033=EDGE_CURVE('',#1681,#1687,#1059,.T.);
#2034=EDGE_CURVE('',#1679,#1688,#1060,.T.);
#2035=EDGE_CURVE('',#1693,#1693,#1507,.F.);
#2036=EDGE_CURVE('',#1693,#1694,#1061,.T.);
#2037=EDGE_CURVE('',#1694,#1694,#1508,.F.);
#2038=EDGE_CURVE('',#1680,#1689,#1062,.T.);
#2039=EDGE_CURVE('',#1685,#1690,#1063,.T.);
#2040=EDGE_CURVE('',#1695,#1695,#1509,.T.);
#2041=EDGE_CURVE('',#1695,#1696,#1064,.T.);
#2042=EDGE_CURVE('',#1696,#1696,#1510,.T.);
#2043=EDGE_CURVE('',#1697,#1697,#1511,.T.);
#2044=EDGE_CURVE('',#1697,#1698,#1065,.T.);
#2045=EDGE_CURVE('',#1698,#1698,#1512,.T.);
#2046=EDGE_CURVE('',#1699,#1699,#1513,.T.);
#2047=EDGE_CURVE('',#1699,#1700,#1066,.T.);
#2048=EDGE_CURVE('',#1700,#1700,#1514,.T.);
#2049=EDGE_CURVE('',#1701,#1701,#1515,.T.);
#2050=EDGE_CURVE('',#1701,#1702,#1067,.T.);
#2051=EDGE_CURVE('',#1702,#1702,#1516,.T.);
#2052=EDGE_CURVE('',#1703,#1704,#1068,.T.);
#2053=EDGE_CURVE('',#1703,#1705,#1517,.T.);
#2054=EDGE_CURVE('',#1706,#1705,#1069,.T.);
#2055=EDGE_CURVE('',#1704,#1706,#1518,.T.);
#2056=EDGE_CURVE('',#1706,#1707,#1070,.T.);
#2057=EDGE_CURVE('',#1708,#1707,#1071,.T.);
#2058=EDGE_CURVE('',#1709,#1708,#1072,.T.);
#2059=EDGE_CURVE('',#1709,#1710,#1073,.T.);
#2060=EDGE_CURVE('',#1710,#1704,#1074,.T.);
#2061=EDGE_CURVE('',#1711,#1705,#1075,.T.);
#2062=EDGE_CURVE('',#1707,#1711,#1076,.T.);
#2063=EDGE_CURVE('',#1703,#1712,#1077,.T.);
#2064=EDGE_CURVE('',#1712,#1713,#1078,.T.);
#2065=EDGE_CURVE('',#1714,#1713,#1079,.T.);
#2066=EDGE_CURVE('',#1711,#1714,#1080,.T.);
#2067=EDGE_CURVE('',#1712,#1710,#1081,.T.);
#2068=EDGE_CURVE('',#1713,#1709,#1082,.T.);
#2069=EDGE_CURVE('',#1715,#1708,#1083,.T.);
#2070=EDGE_CURVE('',#1716,#1715,#1084,.T.);
#2071=EDGE_CURVE('',#1716,#1717,#1085,.T.);
#2072=EDGE_CURVE('',#1717,#1718,#1086,.T.);
#2073=EDGE_CURVE('',#1719,#1718,#1087,.T.);
#2074=EDGE_CURVE('',#1719,#1720,#1088,.T.);
#2075=EDGE_CURVE('',#1720,#1721,#1089,.T.);
#2076=EDGE_CURVE('',#1721,#1722,#1090,.T.);
#2077=EDGE_CURVE('',#1714,#1722,#1091,.T.);
#2078=EDGE_CURVE('',#1723,#1724,#1092,.T.);
#2079=EDGE_CURVE('',#1723,#1725,#1519,.T.);
#2080=EDGE_CURVE('',#1726,#1725,#1093,.T.);
#2081=EDGE_CURVE('',#1724,#1726,#1520,.T.);
#2082=EDGE_CURVE('',#1726,#1727,#1094,.T.);
#2083=EDGE_CURVE('',#1722,#1727,#1095,.T.);
#2084=EDGE_CURVE('',#1721,#1728,#1096,.T.);
#2085=EDGE_CURVE('',#1728,#1724,#1097,.T.);
#2086=EDGE_CURVE('',#1729,#1725,#1098,.T.);
#2087=EDGE_CURVE('',#1727,#1729,#1099,.T.);
#2088=EDGE_CURVE('',#1723,#1730,#1100,.T.);
#2089=EDGE_CURVE('',#1730,#1720,#1101,.T.);
#2090=EDGE_CURVE('',#1729,#1719,#1102,.T.);
#2091=EDGE_CURVE('',#1730,#1728,#1103,.T.);
#2092=EDGE_CURVE('',#1731,#1716,#1104,.T.);
#2093=EDGE_CURVE('',#1732,#1715,#1105,.T.);
#2094=EDGE_CURVE('',#1731,#1732,#1106,.T.);
#2095=EDGE_CURVE('',#1733,#1731,#1107,.T.);
#2096=EDGE_CURVE('',#1734,#1732,#1108,.T.);
#2097=EDGE_CURVE('',#1733,#1734,#1109,.T.);
#2098=EDGE_CURVE('',#1717,#1733,#1110,.T.);
#2099=EDGE_CURVE('',#1718,#1734,#1111,.T.);
#2100=EDGE_CURVE('',#1735,#1735,#1521,.T.);
#2101=EDGE_CURVE('',#1735,#1736,#1112,.T.);
#2102=EDGE_CURVE('',#1737,#1736,#1522,.T.);
#2103=EDGE_CURVE('',#1738,#1737,#301,.T.);
#2104=EDGE_CURVE('',#1736,#1738,#1523,.T.);
#2105=EDGE_CURVE('',#1739,#1740,#302,.T.);
#2106=EDGE_CURVE('',#1741,#1739,#1524,.T.);
#2107=EDGE_CURVE('',#1741,#1742,#1113,.T.);
#2108=EDGE_CURVE('',#1742,#1742,#1525,.T.);
#2109=EDGE_CURVE('',#1740,#1741,#1526,.T.);
#2110=EDGE_CURVE('',#1743,#1744,#1527,.T.);
#2111=EDGE_CURVE('',#1745,#1743,#303,.T.);
#2112=EDGE_CURVE('',#1745,#1746,#1114,.T.);
#2113=EDGE_CURVE('',#1746,#1746,#1528,.T.);
#2114=EDGE_CURVE('',#1744,#1745,#304,.T.);
#2115=EDGE_CURVE('',#1747,#1747,#1529,.T.);
#2116=EDGE_CURVE('',#1747,#1748,#1115,.T.);
#2117=EDGE_CURVE('',#1749,#1748,#305,.T.);
#2118=EDGE_CURVE('',#1750,#1749,#1530,.T.);
#2119=EDGE_CURVE('',#1748,#1750,#306,.T.);
#2120=EDGE_CURVE('',#1739,#1751,#1116,.T.);
#2121=EDGE_CURVE('',#1752,#1751,#1531,.T.);
#2122=EDGE_CURVE('',#1752,#1740,#1117,.T.);
#2123=EDGE_CURVE('',#1738,#1753,#1118,.T.);
#2124=EDGE_CURVE('',#1753,#1754,#1532,.T.);
#2125=EDGE_CURVE('',#1754,#1737,#1119,.T.);
#2126=EDGE_CURVE('',#1755,#1750,#1120,.T.);
#2127=EDGE_CURVE('',#1756,#1755,#1121,.T.);
#2128=EDGE_CURVE('',#1756,#1757,#1122,.T.);
#2129=EDGE_CURVE('',#1757,#1758,#1123,.T.);
#2130=EDGE_CURVE('',#1759,#1758,#307,.T.);
#2131=EDGE_CURVE('',#1760,#1759,#1124,.T.);
#2132=EDGE_CURVE('',#1749,#1760,#1125,.T.);
#2133=EDGE_CURVE('',#1743,#1761,#1126,.T.);
#2134=EDGE_CURVE('',#1762,#1761,#1127,.T.);
#2135=EDGE_CURVE('',#1763,#1762,#308,.T.);
#2136=EDGE_CURVE('',#1764,#1763,#1128,.T.);
#2137=EDGE_CURVE('',#1764,#1765,#1129,.T.);
#2138=EDGE_CURVE('',#1765,#1766,#1130,.T.);
#2139=EDGE_CURVE('',#1766,#1744,#1131,.T.);
#2140=EDGE_CURVE('',#1767,#1768,#1132,.T.);
#2141=EDGE_CURVE('',#1769,#1767,#1133,.T.);
#2142=EDGE_CURVE('',#1770,#1769,#1134,.T.);
#2143=EDGE_CURVE('',#1770,#1768,#1135,.T.);
#2144=EDGE_CURVE('',#1771,#1772,#1136,.T.);
#2145=EDGE_CURVE('',#1771,#1773,#1137,.T.);
#2146=EDGE_CURVE('',#1774,#1773,#1138,.T.);
#2147=EDGE_CURVE('',#1772,#1774,#1139,.T.);
#2148=EDGE_CURVE('',#1772,#1767,#1140,.T.);
#2149=EDGE_CURVE('',#1769,#1774,#1141,.T.);
#2150=EDGE_CURVE('',#1775,#1776,#1533,.T.);
#2151=EDGE_CURVE('',#1776,#1775,#1534,.T.);
#2152=EDGE_CURVE('',#1755,#1775,#1142,.T.);
#2153=EDGE_CURVE('',#1760,#1755,#1535,.T.);
#2154=EDGE_CURVE('',#1776,#1760,#1143,.T.);
#2155=EDGE_CURVE('',#1775,#1776,#309,.T.);
#2156=EDGE_CURVE('',#1777,#1752,#1144,.T.);
#2157=EDGE_CURVE('',#1777,#1770,#1145,.T.);
#2158=EDGE_CURVE('',#1773,#1778,#1146,.T.);
#2159=EDGE_CURVE('',#1778,#1775,#1147,.T.);
#2160=EDGE_CURVE('',#1751,#1776,#1148,.T.);
#2161=EDGE_CURVE('',#1778,#1756,#1149,.T.);
#2162=EDGE_CURVE('',#1758,#1752,#1150,.T.);
#2163=EDGE_CURVE('',#1757,#1777,#1151,.T.);
#2164=EDGE_CURVE('',#1751,#1759,#1152,.T.);
#2165=EDGE_CURVE('',#1759,#1758,#1536,.T.);
#2166=EDGE_CURVE('',#1758,#1759,#1537,.T.);
#2167=EDGE_CURVE('',#1779,#1754,#1153,.T.);
#2168=EDGE_CURVE('',#1779,#1780,#310,.T.);
#2169=EDGE_CURVE('',#1781,#1780,#1154,.T.);
#2170=EDGE_CURVE('',#1781,#1771,#1155,.T.);
#2171=EDGE_CURVE('',#1768,#1782,#1156,.T.);
#2172=EDGE_CURVE('',#1782,#1753,#1157,.T.);
#2173=EDGE_CURVE('',#1779,#1780,#1538,.T.);
#2174=EDGE_CURVE('',#1780,#1779,#1539,.T.);
#2175=EDGE_CURVE('',#1780,#1766,#1158,.T.);
#2176=EDGE_CURVE('',#1761,#1779,#1159,.T.);
#2177=EDGE_CURVE('',#1761,#1766,#1540,.T.);
#2178=EDGE_CURVE('',#1765,#1781,#1160,.T.);
#2179=EDGE_CURVE('',#1753,#1763,#1161,.T.);
#2180=EDGE_CURVE('',#1782,#1764,#1162,.T.);
#2181=EDGE_CURVE('',#1762,#1754,#1163,.T.);
#2182=EDGE_CURVE('',#1762,#1763,#1541,.T.);
#2183=EDGE_CURVE('',#1763,#1762,#1542,.T.);
#2184=EDGE_CURVE('',#1783,#1783,#1543,.T.);
#2185=EDGE_CURVE('',#1783,#1784,#1164,.T.);
#2186=EDGE_CURVE('',#1784,#1784,#1544,.T.);
#2187=EDGE_CURVE('',#1785,#1785,#1545,.T.);
#2188=EDGE_CURVE('',#1785,#1786,#1165,.T.);
#2189=EDGE_CURVE('',#1786,#1786,#1546,.T.);
#2190=EDGE_CURVE('',#1787,#1787,#1547,.T.);
#2191=EDGE_CURVE('',#1788,#1788,#1548,.T.);
#2192=EDGE_CURVE('',#1787,#1789,#1166,.T.);
#2193=EDGE_CURVE('',#1789,#1789,#1549,.T.);
#2194=EDGE_CURVE('',#1790,#1790,#1550,.F.);
#2195=EDGE_CURVE('',#1790,#1791,#1167,.T.);
#2196=EDGE_CURVE('',#1791,#1791,#1551,.F.);
#2197=EDGE_CURVE('',#1788,#1790,#1168,.T.);
#2198=EDGE_CURVE('',#1792,#1792,#1552,.T.);
#2199=EDGE_CURVE('',#1792,#1793,#1169,.T.);
#2200=EDGE_CURVE('',#1794,#1793,#265,.T.);
#2201=EDGE_CURVE('',#1795,#1794,#266,.T.);
#2202=EDGE_CURVE('',#1796,#1795,#267,.T.);
#2203=EDGE_CURVE('',#1797,#1796,#268,.T.);
#2204=EDGE_CURVE('',#1798,#1797,#269,.T.);
#2205=EDGE_CURVE('',#1793,#1798,#270,.T.);
#2206=EDGE_CURVE('',#1799,#1797,#1170,.T.);
#2207=EDGE_CURVE('',#1799,#1800,#1171,.T.);
#2208=EDGE_CURVE('',#1800,#1798,#1172,.T.);
#2209=EDGE_CURVE('',#1801,#1796,#1173,.T.);
#2210=EDGE_CURVE('',#1801,#1799,#1174,.T.);
#2211=EDGE_CURVE('',#1802,#1795,#1175,.T.);
#2212=EDGE_CURVE('',#1802,#1801,#1176,.T.);
#2213=EDGE_CURVE('',#1803,#1794,#1177,.T.);
#2214=EDGE_CURVE('',#1803,#1802,#1178,.T.);
#2215=EDGE_CURVE('',#1804,#1793,#1179,.T.);
#2216=EDGE_CURVE('',#1804,#1803,#1180,.T.);
#2217=EDGE_CURVE('',#1800,#1804,#1181,.T.);
#2218=EDGE_CURVE('',#1805,#1805,#1553,.T.);
#2219=EDGE_CURVE('',#1805,#1806,#1182,.T.);
#2220=EDGE_CURVE('',#1806,#1806,#1554,.T.);
#2221=EDGE_CURVE('',#1807,#1807,#1555,.T.);
#2222=EDGE_CURVE('',#1807,#1808,#1183,.T.);
#2223=EDGE_CURVE('',#1808,#1808,#1556,.T.);
#2224=EDGE_CURVE('',#1809,#1810,#271,.T.);
#2225=EDGE_CURVE('',#1811,#1809,#272,.T.);
#2226=EDGE_CURVE('',#1811,#1812,#1184,.T.);
#2227=EDGE_CURVE('',#1812,#1812,#1557,.T.);
#2228=EDGE_CURVE('',#1813,#1811,#273,.T.);
#2229=EDGE_CURVE('',#1814,#1813,#274,.T.);
#2230=EDGE_CURVE('',#1815,#1814,#275,.T.);
#2231=EDGE_CURVE('',#1810,#1815,#276,.T.);
#2232=EDGE_CURVE('',#1816,#1816,#1558,.T.);
#2233=EDGE_CURVE('',#1816,#1817,#1185,.T.);
#2234=EDGE_CURVE('',#1818,#1817,#277,.T.);
#2235=EDGE_CURVE('',#1819,#1818,#278,.T.);
#2236=EDGE_CURVE('',#1820,#1819,#279,.T.);
#2237=EDGE_CURVE('',#1821,#1820,#280,.T.);
#2238=EDGE_CURVE('',#1822,#1821,#281,.T.);
#2239=EDGE_CURVE('',#1817,#1822,#282,.T.);
#2240=EDGE_CURVE('',#1813,#1822,#1186,.T.);
#2241=EDGE_CURVE('',#1814,#1821,#1187,.T.);
#2242=EDGE_CURVE('',#1811,#1817,#1188,.T.);
#2243=EDGE_CURVE('',#1809,#1818,#1189,.T.);
#2244=EDGE_CURVE('',#1823,#1823,#1559,.F.);
#2245=EDGE_CURVE('',#1823,#1824,#1190,.T.);
#2246=EDGE_CURVE('',#1824,#1824,#1560,.F.);
#2247=EDGE_CURVE('',#1810,#1819,#1191,.T.);
#2248=EDGE_CURVE('',#1815,#1820,#1192,.T.);
#2249=ORIENTED_EDGE('',*,*,#1825,.F.);
#2250=ORIENTED_EDGE('',*,*,#1826,.T.);
#2251=ORIENTED_EDGE('',*,*,#1827,.F.);
#2252=ORIENTED_EDGE('',*,*,#1826,.F.);
#2253=ORIENTED_EDGE('',*,*,#1828,.F.);
#2254=ORIENTED_EDGE('',*,*,#1829,.T.);
#2255=ORIENTED_EDGE('',*,*,#1830,.F.);
#2256=ORIENTED_EDGE('',*,*,#1829,.F.);
#2257=ORIENTED_EDGE('',*,*,#1831,.F.);
#2258=ORIENTED_EDGE('',*,*,#1832,.T.);
#2259=ORIENTED_EDGE('',*,*,#1833,.F.);
#2260=ORIENTED_EDGE('',*,*,#1832,.F.);
#2261=ORIENTED_EDGE('',*,*,#1834,.F.);
#2262=ORIENTED_EDGE('',*,*,#1835,.T.);
#2263=ORIENTED_EDGE('',*,*,#1836,.F.);
#2264=ORIENTED_EDGE('',*,*,#1835,.F.);
#2265=ORIENTED_EDGE('',*,*,#1837,.F.);
#2266=ORIENTED_EDGE('',*,*,#1838,.T.);
#2267=ORIENTED_EDGE('',*,*,#1839,.F.);
#2268=ORIENTED_EDGE('',*,*,#1840,.F.);
#2269=ORIENTED_EDGE('',*,*,#1840,.T.);
#2270=ORIENTED_EDGE('',*,*,#1841,.T.);
#2271=ORIENTED_EDGE('',*,*,#1842,.T.);
#2272=ORIENTED_EDGE('',*,*,#1843,.F.);
#2273=ORIENTED_EDGE('',*,*,#1844,.F.);
#2274=ORIENTED_EDGE('',*,*,#1845,.T.);
#2275=ORIENTED_EDGE('',*,*,#1836,.T.);
#2276=ORIENTED_EDGE('',*,*,#1839,.T.);
#2277=ORIENTED_EDGE('',*,*,#1846,.F.);
#2278=ORIENTED_EDGE('',*,*,#1847,.T.);
#2279=ORIENTED_EDGE('',*,*,#1841,.F.);
#2280=ORIENTED_EDGE('',*,*,#1848,.T.);
#2281=ORIENTED_EDGE('',*,*,#1849,.F.);
#2282=ORIENTED_EDGE('',*,*,#1850,.F.);
#2283=ORIENTED_EDGE('',*,*,#1851,.T.);
#2284=ORIENTED_EDGE('',*,*,#1846,.T.);
#2285=ORIENTED_EDGE('',*,*,#1838,.F.);
#2286=ORIENTED_EDGE('',*,*,#1834,.T.);
#2287=ORIENTED_EDGE('',*,*,#1852,.F.);
#2288=ORIENTED_EDGE('',*,*,#1842,.F.);
#2289=ORIENTED_EDGE('',*,*,#1847,.F.);
#2290=ORIENTED_EDGE('',*,*,#1851,.F.);
#2291=ORIENTED_EDGE('',*,*,#1837,.T.);
#2292=ORIENTED_EDGE('',*,*,#1845,.F.);
#2293=ORIENTED_EDGE('',*,*,#1853,.F.);
#2294=ORIENTED_EDGE('',*,*,#1848,.F.);
#2295=ORIENTED_EDGE('',*,*,#1849,.T.);
#2296=ORIENTED_EDGE('',*,*,#1853,.T.);
#2297=ORIENTED_EDGE('',*,*,#1844,.T.);
#2298=ORIENTED_EDGE('',*,*,#1854,.T.);
#2299=ORIENTED_EDGE('',*,*,#1855,.T.);
#2300=ORIENTED_EDGE('',*,*,#1856,.T.);
#2301=ORIENTED_EDGE('',*,*,#1857,.T.);
#2302=ORIENTED_EDGE('',*,*,#1858,.T.);
#2303=ORIENTED_EDGE('',*,*,#1859,.T.);
#2304=ORIENTED_EDGE('',*,*,#1860,.T.);
#2305=ORIENTED_EDGE('',*,*,#1861,.T.);
#2306=ORIENTED_EDGE('',*,*,#1862,.T.);
#2307=ORIENTED_EDGE('',*,*,#1827,.T.);
#2308=ORIENTED_EDGE('',*,*,#1830,.T.);
#2309=ORIENTED_EDGE('',*,*,#1863,.F.);
#2310=ORIENTED_EDGE('',*,*,#1864,.T.);
#2311=ORIENTED_EDGE('',*,*,#1865,.F.);
#2312=ORIENTED_EDGE('',*,*,#1866,.F.);
#2313=ORIENTED_EDGE('',*,*,#1866,.T.);
#2314=ORIENTED_EDGE('',*,*,#1867,.T.);
#2315=ORIENTED_EDGE('',*,*,#1868,.T.);
#2316=ORIENTED_EDGE('',*,*,#1869,.F.);
#2317=ORIENTED_EDGE('',*,*,#1861,.F.);
#2318=ORIENTED_EDGE('',*,*,#1870,.T.);
#2319=ORIENTED_EDGE('',*,*,#1833,.T.);
#2320=ORIENTED_EDGE('',*,*,#1865,.T.);
#2321=ORIENTED_EDGE('',*,*,#1871,.F.);
#2322=ORIENTED_EDGE('',*,*,#1872,.T.);
#2323=ORIENTED_EDGE('',*,*,#1867,.F.);
#2324=ORIENTED_EDGE('',*,*,#1873,.T.);
#2325=ORIENTED_EDGE('',*,*,#1859,.F.);
#2326=ORIENTED_EDGE('',*,*,#1874,.F.);
#2327=ORIENTED_EDGE('',*,*,#1875,.T.);
#2328=ORIENTED_EDGE('',*,*,#1871,.T.);
#2329=ORIENTED_EDGE('',*,*,#1864,.F.);
#2330=ORIENTED_EDGE('',*,*,#1831,.T.);
#2331=ORIENTED_EDGE('',*,*,#1876,.F.);
#2332=ORIENTED_EDGE('',*,*,#1868,.F.);
#2333=ORIENTED_EDGE('',*,*,#1872,.F.);
#2334=ORIENTED_EDGE('',*,*,#1875,.F.);
#2335=ORIENTED_EDGE('',*,*,#1863,.T.);
#2336=ORIENTED_EDGE('',*,*,#1870,.F.);
#2337=ORIENTED_EDGE('',*,*,#1860,.F.);
#2338=ORIENTED_EDGE('',*,*,#1873,.F.);
#2339=ORIENTED_EDGE('',*,*,#1877,.T.);
#2340=ORIENTED_EDGE('',*,*,#1878,.T.);
#2341=ORIENTED_EDGE('',*,*,#1855,.F.);
#2342=ORIENTED_EDGE('',*,*,#1879,.F.);
#2343=ORIENTED_EDGE('',*,*,#1850,.T.);
#2344=ORIENTED_EDGE('',*,*,#1862,.F.);
#2345=ORIENTED_EDGE('',*,*,#1869,.T.);
#2346=ORIENTED_EDGE('',*,*,#1876,.T.);
#2347=ORIENTED_EDGE('',*,*,#1874,.T.);
#2348=ORIENTED_EDGE('',*,*,#1858,.F.);
#2349=ORIENTED_EDGE('',*,*,#1880,.F.);
#2350=ORIENTED_EDGE('',*,*,#1881,.T.);
#2351=ORIENTED_EDGE('',*,*,#1879,.T.);
#2352=ORIENTED_EDGE('',*,*,#1854,.F.);
#2353=ORIENTED_EDGE('',*,*,#1843,.T.);
#2354=ORIENTED_EDGE('',*,*,#1852,.T.);
#2355=ORIENTED_EDGE('',*,*,#1882,.T.);
#2356=ORIENTED_EDGE('',*,*,#1880,.T.);
#2357=ORIENTED_EDGE('',*,*,#1857,.F.);
#2358=ORIENTED_EDGE('',*,*,#1883,.F.);
#2359=ORIENTED_EDGE('',*,*,#1884,.T.);
#2360=ORIENTED_EDGE('',*,*,#1883,.T.);
#2361=ORIENTED_EDGE('',*,*,#1856,.F.);
#2362=ORIENTED_EDGE('',*,*,#1878,.F.);
#2363=ORIENTED_EDGE('',*,*,#1884,.F.);
#2364=ORIENTED_EDGE('',*,*,#1877,.F.);
#2365=ORIENTED_EDGE('',*,*,#1881,.F.);
#2366=ORIENTED_EDGE('',*,*,#1882,.F.);
#2367=ORIENTED_EDGE('',*,*,#1825,.T.);
#2368=ORIENTED_EDGE('',*,*,#1828,.T.);
#2369=ORIENTED_EDGE('',*,*,#1885,.F.);
#2370=ORIENTED_EDGE('',*,*,#1886,.T.);
#2371=ORIENTED_EDGE('',*,*,#1887,.F.);
#2372=ORIENTED_EDGE('',*,*,#1888,.F.);
#2373=ORIENTED_EDGE('',*,*,#1889,.F.);
#2374=ORIENTED_EDGE('',*,*,#1886,.F.);
#2375=ORIENTED_EDGE('',*,*,#1890,.F.);
#2376=ORIENTED_EDGE('',*,*,#1891,.F.);
#2377=ORIENTED_EDGE('',*,*,#1892,.T.);
#2378=ORIENTED_EDGE('',*,*,#1893,.F.);
#2379=ORIENTED_EDGE('',*,*,#1892,.F.);
#2380=ORIENTED_EDGE('',*,*,#1894,.F.);
#2381=ORIENTED_EDGE('',*,*,#1895,.F.);
#2382=ORIENTED_EDGE('',*,*,#1896,.F.);
#2383=ORIENTED_EDGE('',*,*,#1897,.T.);
#2384=ORIENTED_EDGE('',*,*,#1898,.F.);
#2385=ORIENTED_EDGE('',*,*,#1897,.F.);
#2386=ORIENTED_EDGE('',*,*,#1899,.F.);
#2387=ORIENTED_EDGE('',*,*,#1900,.F.);
#2388=ORIENTED_EDGE('',*,*,#1901,.T.);
#2389=ORIENTED_EDGE('',*,*,#1902,.F.);
#2390=ORIENTED_EDGE('',*,*,#1903,.F.);
#2391=ORIENTED_EDGE('',*,*,#1904,.F.);
#2392=ORIENTED_EDGE('',*,*,#1901,.F.);
#2393=ORIENTED_EDGE('',*,*,#1894,.T.);
#2394=ORIENTED_EDGE('',*,*,#1891,.T.);
#2395=ORIENTED_EDGE('',*,*,#1905,.T.);
#2396=ORIENTED_EDGE('',*,*,#1906,.F.);
#2397=ORIENTED_EDGE('',*,*,#1907,.T.);
#2398=ORIENTED_EDGE('',*,*,#1887,.T.);
#2399=ORIENTED_EDGE('',*,*,#1889,.T.);
#2400=ORIENTED_EDGE('',*,*,#1908,.T.);
#2401=ORIENTED_EDGE('',*,*,#1909,.T.);
#2402=ORIENTED_EDGE('',*,*,#1910,.T.);
#2403=ORIENTED_EDGE('',*,*,#1902,.T.);
#2404=ORIENTED_EDGE('',*,*,#1904,.T.);
#2405=ORIENTED_EDGE('',*,*,#1911,.F.);
#2406=ORIENTED_EDGE('',*,*,#1912,.F.);
#2407=ORIENTED_EDGE('',*,*,#1913,.T.);
#2408=ORIENTED_EDGE('',*,*,#1914,.T.);
#2409=ORIENTED_EDGE('',*,*,#1915,.F.);
#2410=ORIENTED_EDGE('',*,*,#1916,.F.);
#2411=ORIENTED_EDGE('',*,*,#1917,.F.);
#2412=ORIENTED_EDGE('',*,*,#1899,.T.);
#2413=ORIENTED_EDGE('',*,*,#1896,.T.);
#2414=ORIENTED_EDGE('',*,*,#1918,.T.);
#2415=ORIENTED_EDGE('',*,*,#1919,.F.);
#2416=ORIENTED_EDGE('',*,*,#1920,.F.);
#2417=ORIENTED_EDGE('',*,*,#1921,.F.);
#2418=ORIENTED_EDGE('',*,*,#1922,.T.);
#2419=ORIENTED_EDGE('',*,*,#1923,.T.);
#2420=ORIENTED_EDGE('',*,*,#1924,.T.);
#2421=ORIENTED_EDGE('',*,*,#1925,.F.);
#2422=ORIENTED_EDGE('',*,*,#1926,.F.);
#2423=ORIENTED_EDGE('',*,*,#1927,.F.);
#2424=ORIENTED_EDGE('',*,*,#1928,.T.);
#2425=ORIENTED_EDGE('',*,*,#1929,.F.);
#2426=ORIENTED_EDGE('',*,*,#1930,.T.);
#2427=ORIENTED_EDGE('',*,*,#1931,.F.);
#2428=ORIENTED_EDGE('',*,*,#1932,.F.);
#2429=ORIENTED_EDGE('',*,*,#1933,.F.);
#2430=ORIENTED_EDGE('',*,*,#1932,.T.);
#2431=ORIENTED_EDGE('',*,*,#1934,.F.);
#2432=ORIENTED_EDGE('',*,*,#1926,.T.);
#2433=ORIENTED_EDGE('',*,*,#1935,.F.);
#2434=ORIENTED_EDGE('',*,*,#1936,.F.);
#2435=ORIENTED_EDGE('',*,*,#1900,.T.);
#2436=ORIENTED_EDGE('',*,*,#1937,.F.);
#2437=ORIENTED_EDGE('',*,*,#1938,.F.);
#2438=ORIENTED_EDGE('',*,*,#1939,.F.);
#2439=ORIENTED_EDGE('',*,*,#1936,.T.);
#2440=ORIENTED_EDGE('',*,*,#1903,.T.);
#2441=ORIENTED_EDGE('',*,*,#1917,.T.);
#2442=ORIENTED_EDGE('',*,*,#1938,.T.);
#2443=ORIENTED_EDGE('',*,*,#1911,.T.);
#2444=ORIENTED_EDGE('',*,*,#1940,.F.);
#2445=ORIENTED_EDGE('',*,*,#1935,.T.);
#2446=ORIENTED_EDGE('',*,*,#1890,.T.);
#2447=ORIENTED_EDGE('',*,*,#1907,.F.);
#2448=ORIENTED_EDGE('',*,*,#1941,.F.);
#2449=ORIENTED_EDGE('',*,*,#1942,.T.);
#2450=ORIENTED_EDGE('',*,*,#1927,.T.);
#2451=ORIENTED_EDGE('',*,*,#1934,.T.);
#2452=ORIENTED_EDGE('',*,*,#1931,.T.);
#2453=ORIENTED_EDGE('',*,*,#1943,.T.);
#2454=ORIENTED_EDGE('',*,*,#1944,.T.);
#2455=ORIENTED_EDGE('',*,*,#1940,.T.);
#2456=ORIENTED_EDGE('',*,*,#1945,.F.);
#2457=ORIENTED_EDGE('',*,*,#1905,.F.);
#2458=ORIENTED_EDGE('',*,*,#1937,.T.);
#2459=ORIENTED_EDGE('',*,*,#1944,.F.);
#2460=ORIENTED_EDGE('',*,*,#1946,.T.);
#2461=ORIENTED_EDGE('',*,*,#1912,.T.);
#2462=ORIENTED_EDGE('',*,*,#1947,.F.);
#2463=ORIENTED_EDGE('',*,*,#1914,.F.);
#2464=ORIENTED_EDGE('',*,*,#1948,.T.);
#2465=ORIENTED_EDGE('',*,*,#1941,.T.);
#2466=ORIENTED_EDGE('',*,*,#1949,.F.);
#2467=ORIENTED_EDGE('',*,*,#1945,.T.);
#2468=ORIENTED_EDGE('',*,*,#1939,.T.);
#2469=ORIENTED_EDGE('',*,*,#1916,.T.);
#2470=ORIENTED_EDGE('',*,*,#1915,.T.);
#2471=ORIENTED_EDGE('',*,*,#1950,.F.);
#2472=ORIENTED_EDGE('',*,*,#1949,.T.);
#2473=ORIENTED_EDGE('',*,*,#1951,.F.);
#2474=ORIENTED_EDGE('',*,*,#1947,.T.);
#2475=ORIENTED_EDGE('',*,*,#1906,.T.);
#2476=ORIENTED_EDGE('',*,*,#1950,.T.);
#2477=ORIENTED_EDGE('',*,*,#1951,.T.);
#2478=ORIENTED_EDGE('',*,*,#1893,.T.);
#2479=ORIENTED_EDGE('',*,*,#1888,.T.);
#2480=ORIENTED_EDGE('',*,*,#1910,.F.);
#2481=ORIENTED_EDGE('',*,*,#1952,.F.);
#2482=ORIENTED_EDGE('',*,*,#1953,.T.);
#2483=ORIENTED_EDGE('',*,*,#1954,.F.);
#2484=ORIENTED_EDGE('',*,*,#1955,.T.);
#2485=ORIENTED_EDGE('',*,*,#1929,.T.);
#2486=ORIENTED_EDGE('',*,*,#1933,.T.);
#2487=ORIENTED_EDGE('',*,*,#1925,.T.);
#2488=ORIENTED_EDGE('',*,*,#1956,.T.);
#2489=ORIENTED_EDGE('',*,*,#1957,.T.);
#2490=ORIENTED_EDGE('',*,*,#1908,.F.);
#2491=ORIENTED_EDGE('',*,*,#1958,.T.);
#2492=ORIENTED_EDGE('',*,*,#1959,.T.);
#2493=ORIENTED_EDGE('',*,*,#1898,.T.);
#2494=ORIENTED_EDGE('',*,*,#1953,.F.);
#2495=ORIENTED_EDGE('',*,*,#1959,.F.);
#2496=ORIENTED_EDGE('',*,*,#1960,.F.);
#2497=ORIENTED_EDGE('',*,*,#1958,.F.);
#2498=ORIENTED_EDGE('',*,*,#1961,.F.);
#2499=ORIENTED_EDGE('',*,*,#1962,.T.);
#2500=ORIENTED_EDGE('',*,*,#1895,.T.);
#2501=ORIENTED_EDGE('',*,*,#1924,.F.);
#2502=ORIENTED_EDGE('',*,*,#1962,.F.);
#2503=ORIENTED_EDGE('',*,*,#1918,.F.);
#2504=ORIENTED_EDGE('',*,*,#1960,.T.);
#2505=ORIENTED_EDGE('',*,*,#1923,.F.);
#2506=ORIENTED_EDGE('',*,*,#1963,.T.);
#2507=ORIENTED_EDGE('',*,*,#1954,.T.);
#2508=ORIENTED_EDGE('',*,*,#1964,.F.);
#2509=ORIENTED_EDGE('',*,*,#1957,.F.);
#2510=ORIENTED_EDGE('',*,*,#1965,.T.);
#2511=ORIENTED_EDGE('',*,*,#1921,.T.);
#2512=ORIENTED_EDGE('',*,*,#1966,.F.);
#2513=ORIENTED_EDGE('',*,*,#1919,.T.);
#2514=ORIENTED_EDGE('',*,*,#1961,.T.);
#2515=ORIENTED_EDGE('',*,*,#1952,.T.);
#2516=ORIENTED_EDGE('',*,*,#1955,.F.);
#2517=ORIENTED_EDGE('',*,*,#1963,.F.);
#2518=ORIENTED_EDGE('',*,*,#1922,.F.);
#2519=ORIENTED_EDGE('',*,*,#1965,.F.);
#2520=ORIENTED_EDGE('',*,*,#1956,.F.);
#2521=ORIENTED_EDGE('',*,*,#1928,.F.);
#2522=ORIENTED_EDGE('',*,*,#1942,.F.);
#2523=ORIENTED_EDGE('',*,*,#1948,.F.);
#2524=ORIENTED_EDGE('',*,*,#1913,.F.);
#2525=ORIENTED_EDGE('',*,*,#1946,.F.);
#2526=ORIENTED_EDGE('',*,*,#1943,.F.);
#2527=ORIENTED_EDGE('',*,*,#1930,.F.);
#2528=ORIENTED_EDGE('',*,*,#1967,.F.);
#2529=ORIENTED_EDGE('',*,*,#1968,.F.);
#2530=ORIENTED_EDGE('',*,*,#1885,.T.);
#2531=ORIENTED_EDGE('',*,*,#1920,.T.);
#2532=ORIENTED_EDGE('',*,*,#1967,.T.);
#2533=ORIENTED_EDGE('',*,*,#1964,.T.);
#2534=ORIENTED_EDGE('',*,*,#1968,.T.);
#2535=ORIENTED_EDGE('',*,*,#1966,.T.);
#2536=ORIENTED_EDGE('',*,*,#1909,.F.);
#2537=ORIENTED_EDGE('',*,*,#1969,.F.);
#2538=ORIENTED_EDGE('',*,*,#1970,.T.);
#2539=ORIENTED_EDGE('',*,*,#1971,.T.);
#2540=ORIENTED_EDGE('',*,*,#1970,.F.);
#2541=ORIENTED_EDGE('',*,*,#1972,.F.);
#2542=ORIENTED_EDGE('',*,*,#1973,.T.);
#2543=ORIENTED_EDGE('',*,*,#1974,.T.);
#2544=ORIENTED_EDGE('',*,*,#1973,.F.);
#2545=ORIENTED_EDGE('',*,*,#1972,.T.);
#2546=ORIENTED_EDGE('',*,*,#1969,.T.);
#2547=ORIENTED_EDGE('',*,*,#1974,.F.);
#2548=ORIENTED_EDGE('',*,*,#1971,.F.);
#2549=ORIENTED_EDGE('',*,*,#1975,.T.);
#2550=ORIENTED_EDGE('',*,*,#1976,.F.);
#2551=ORIENTED_EDGE('',*,*,#1975,.F.);
#2552=ORIENTED_EDGE('',*,*,#1977,.T.);
#2553=ORIENTED_EDGE('',*,*,#1978,.T.);
#2554=ORIENTED_EDGE('',*,*,#1977,.F.);
#2555=ORIENTED_EDGE('',*,*,#1978,.F.);
#2556=ORIENTED_EDGE('',*,*,#1979,.F.);
#2557=ORIENTED_EDGE('',*,*,#1980,.T.);
#2558=ORIENTED_EDGE('',*,*,#1981,.F.);
#2559=ORIENTED_EDGE('',*,*,#1980,.F.);
#2560=ORIENTED_EDGE('',*,*,#1976,.T.);
#2561=ORIENTED_EDGE('',*,*,#1982,.T.);
#2562=ORIENTED_EDGE('',*,*,#1979,.T.);
#2563=ORIENTED_EDGE('',*,*,#1982,.F.);
#2564=ORIENTED_EDGE('',*,*,#1983,.F.);
#2565=ORIENTED_EDGE('',*,*,#1984,.T.);
#2566=ORIENTED_EDGE('',*,*,#1985,.F.);
#2567=ORIENTED_EDGE('',*,*,#1986,.F.);
#2568=ORIENTED_EDGE('',*,*,#1987,.F.);
#2569=ORIENTED_EDGE('',*,*,#1988,.F.);
#2570=ORIENTED_EDGE('',*,*,#1989,.F.);
#2571=ORIENTED_EDGE('',*,*,#1990,.F.);
#2572=ORIENTED_EDGE('',*,*,#1984,.F.);
#2573=ORIENTED_EDGE('',*,*,#1989,.T.);
#2574=ORIENTED_EDGE('',*,*,#1991,.F.);
#2575=ORIENTED_EDGE('',*,*,#1992,.T.);
#2576=ORIENTED_EDGE('',*,*,#1993,.T.);
#2577=ORIENTED_EDGE('',*,*,#1988,.T.);
#2578=ORIENTED_EDGE('',*,*,#1994,.F.);
#2579=ORIENTED_EDGE('',*,*,#1995,.T.);
#2580=ORIENTED_EDGE('',*,*,#1991,.T.);
#2581=ORIENTED_EDGE('',*,*,#1987,.T.);
#2582=ORIENTED_EDGE('',*,*,#1996,.F.);
#2583=ORIENTED_EDGE('',*,*,#1997,.T.);
#2584=ORIENTED_EDGE('',*,*,#1994,.T.);
#2585=ORIENTED_EDGE('',*,*,#1986,.T.);
#2586=ORIENTED_EDGE('',*,*,#1998,.F.);
#2587=ORIENTED_EDGE('',*,*,#1999,.T.);
#2588=ORIENTED_EDGE('',*,*,#1996,.T.);
#2589=ORIENTED_EDGE('',*,*,#1985,.T.);
#2590=ORIENTED_EDGE('',*,*,#2000,.F.);
#2591=ORIENTED_EDGE('',*,*,#2001,.T.);
#2592=ORIENTED_EDGE('',*,*,#1998,.T.);
#2593=ORIENTED_EDGE('',*,*,#1990,.T.);
#2594=ORIENTED_EDGE('',*,*,#1993,.F.);
#2595=ORIENTED_EDGE('',*,*,#2002,.T.);
#2596=ORIENTED_EDGE('',*,*,#2000,.T.);
#2597=ORIENTED_EDGE('',*,*,#1983,.T.);
#2598=ORIENTED_EDGE('',*,*,#1997,.F.);
#2599=ORIENTED_EDGE('',*,*,#1999,.F.);
#2600=ORIENTED_EDGE('',*,*,#2001,.F.);
#2601=ORIENTED_EDGE('',*,*,#2002,.F.);
#2602=ORIENTED_EDGE('',*,*,#1992,.F.);
#2603=ORIENTED_EDGE('',*,*,#1995,.F.);
#2604=ORIENTED_EDGE('',*,*,#1981,.T.);
#2605=ORIENTED_EDGE('',*,*,#2003,.F.);
#2606=ORIENTED_EDGE('',*,*,#2004,.T.);
#2607=ORIENTED_EDGE('',*,*,#2005,.T.);
#2608=ORIENTED_EDGE('',*,*,#2004,.F.);
#2609=ORIENTED_EDGE('',*,*,#2006,.F.);
#2610=ORIENTED_EDGE('',*,*,#2007,.T.);
#2611=ORIENTED_EDGE('',*,*,#2008,.T.);
#2612=ORIENTED_EDGE('',*,*,#2007,.F.);
#2613=ORIENTED_EDGE('',*,*,#2006,.T.);
#2614=ORIENTED_EDGE('',*,*,#2003,.T.);
#2615=ORIENTED_EDGE('',*,*,#2008,.F.);
#2616=ORIENTED_EDGE('',*,*,#2005,.F.);
#2617=ORIENTED_EDGE('',*,*,#2009,.F.);
#2618=ORIENTED_EDGE('',*,*,#2010,.T.);
#2619=ORIENTED_EDGE('',*,*,#2011,.T.);
#2620=ORIENTED_EDGE('',*,*,#2010,.F.);
#2621=ORIENTED_EDGE('',*,*,#2012,.F.);
#2622=ORIENTED_EDGE('',*,*,#2013,.T.);
#2623=ORIENTED_EDGE('',*,*,#2014,.T.);
#2624=ORIENTED_EDGE('',*,*,#2013,.F.);
#2625=ORIENTED_EDGE('',*,*,#2012,.T.);
#2626=ORIENTED_EDGE('',*,*,#2009,.T.);
#2627=ORIENTED_EDGE('',*,*,#2014,.F.);
#2628=ORIENTED_EDGE('',*,*,#2011,.F.);
#2629=ORIENTED_EDGE('',*,*,#2015,.F.);
#2630=ORIENTED_EDGE('',*,*,#2016,.F.);
#2631=ORIENTED_EDGE('',*,*,#2017,.T.);
#2632=ORIENTED_EDGE('',*,*,#2018,.F.);
#2633=ORIENTED_EDGE('',*,*,#2017,.F.);
#2634=ORIENTED_EDGE('',*,*,#2019,.F.);
#2635=ORIENTED_EDGE('',*,*,#2020,.F.);
#2636=ORIENTED_EDGE('',*,*,#2021,.F.);
#2637=ORIENTED_EDGE('',*,*,#2022,.F.);
#2638=ORIENTED_EDGE('',*,*,#2023,.F.);
#2639=ORIENTED_EDGE('',*,*,#2024,.T.);
#2640=ORIENTED_EDGE('',*,*,#2025,.F.);
#2641=ORIENTED_EDGE('',*,*,#2026,.F.);
#2642=ORIENTED_EDGE('',*,*,#2027,.F.);
#2643=ORIENTED_EDGE('',*,*,#2028,.F.);
#2644=ORIENTED_EDGE('',*,*,#2029,.F.);
#2645=ORIENTED_EDGE('',*,*,#2030,.F.);
#2646=ORIENTED_EDGE('',*,*,#2024,.F.);
#2647=ORIENTED_EDGE('',*,*,#2020,.T.);
#2648=ORIENTED_EDGE('',*,*,#2031,.T.);
#2649=ORIENTED_EDGE('',*,*,#2029,.T.);
#2650=ORIENTED_EDGE('',*,*,#2032,.F.);
#2651=ORIENTED_EDGE('',*,*,#2019,.T.);
#2652=ORIENTED_EDGE('',*,*,#2033,.T.);
#2653=ORIENTED_EDGE('',*,*,#2030,.T.);
#2654=ORIENTED_EDGE('',*,*,#2031,.F.);
#2655=ORIENTED_EDGE('',*,*,#2016,.T.);
#2656=ORIENTED_EDGE('',*,*,#2034,.T.);
#2657=ORIENTED_EDGE('',*,*,#2025,.T.);
#2658=ORIENTED_EDGE('',*,*,#2033,.F.);
#2659=ORIENTED_EDGE('',*,*,#2035,.F.);
#2660=ORIENTED_EDGE('',*,*,#2036,.T.);
#2661=ORIENTED_EDGE('',*,*,#2037,.T.);
#2662=ORIENTED_EDGE('',*,*,#2036,.F.);
#2663=ORIENTED_EDGE('',*,*,#2015,.T.);
#2664=ORIENTED_EDGE('',*,*,#2038,.T.);
#2665=ORIENTED_EDGE('',*,*,#2026,.T.);
#2666=ORIENTED_EDGE('',*,*,#2034,.F.);
#2667=ORIENTED_EDGE('',*,*,#2021,.T.);
#2668=ORIENTED_EDGE('',*,*,#2032,.T.);
#2669=ORIENTED_EDGE('',*,*,#2028,.T.);
#2670=ORIENTED_EDGE('',*,*,#2039,.F.);
#2671=ORIENTED_EDGE('',*,*,#2022,.T.);
#2672=ORIENTED_EDGE('',*,*,#2039,.T.);
#2673=ORIENTED_EDGE('',*,*,#2027,.T.);
#2674=ORIENTED_EDGE('',*,*,#2038,.F.);
#2675=ORIENTED_EDGE('',*,*,#2023,.T.);
#2676=ORIENTED_EDGE('',*,*,#2035,.T.);
#2677=ORIENTED_EDGE('',*,*,#2018,.T.);
#2678=ORIENTED_EDGE('',*,*,#2037,.F.);
#2679=ORIENTED_EDGE('',*,*,#2040,.F.);
#2680=ORIENTED_EDGE('',*,*,#2041,.T.);
#2681=ORIENTED_EDGE('',*,*,#2042,.F.);
#2682=ORIENTED_EDGE('',*,*,#2041,.F.);
#2683=ORIENTED_EDGE('',*,*,#2043,.F.);
#2684=ORIENTED_EDGE('',*,*,#2044,.T.);
#2685=ORIENTED_EDGE('',*,*,#2045,.F.);
#2686=ORIENTED_EDGE('',*,*,#2044,.F.);
#2687=ORIENTED_EDGE('',*,*,#2046,.F.);
#2688=ORIENTED_EDGE('',*,*,#2047,.T.);
#2689=ORIENTED_EDGE('',*,*,#2048,.F.);
#2690=ORIENTED_EDGE('',*,*,#2047,.F.);
#2691=ORIENTED_EDGE('',*,*,#2049,.F.);
#2692=ORIENTED_EDGE('',*,*,#2050,.T.);
#2693=ORIENTED_EDGE('',*,*,#2051,.F.);
#2694=ORIENTED_EDGE('',*,*,#2050,.F.);
#2695=ORIENTED_EDGE('',*,*,#2052,.F.);
#2696=ORIENTED_EDGE('',*,*,#2053,.T.);
#2697=ORIENTED_EDGE('',*,*,#2054,.F.);
#2698=ORIENTED_EDGE('',*,*,#2055,.F.);
#2699=ORIENTED_EDGE('',*,*,#2055,.T.);
#2700=ORIENTED_EDGE('',*,*,#2056,.T.);
#2701=ORIENTED_EDGE('',*,*,#2057,.F.);
#2702=ORIENTED_EDGE('',*,*,#2058,.F.);
#2703=ORIENTED_EDGE('',*,*,#2059,.T.);
#2704=ORIENTED_EDGE('',*,*,#2060,.T.);
#2705=ORIENTED_EDGE('',*,*,#2051,.T.);
#2706=ORIENTED_EDGE('',*,*,#2054,.T.);
#2707=ORIENTED_EDGE('',*,*,#2061,.F.);
#2708=ORIENTED_EDGE('',*,*,#2062,.F.);
#2709=ORIENTED_EDGE('',*,*,#2056,.F.);
#2710=ORIENTED_EDGE('',*,*,#2063,.T.);
#2711=ORIENTED_EDGE('',*,*,#2064,.T.);
#2712=ORIENTED_EDGE('',*,*,#2065,.F.);
#2713=ORIENTED_EDGE('',*,*,#2066,.F.);
#2714=ORIENTED_EDGE('',*,*,#2061,.T.);
#2715=ORIENTED_EDGE('',*,*,#2053,.F.);
#2716=ORIENTED_EDGE('',*,*,#2049,.T.);
#2717=ORIENTED_EDGE('',*,*,#2052,.T.);
#2718=ORIENTED_EDGE('',*,*,#2060,.F.);
#2719=ORIENTED_EDGE('',*,*,#2067,.F.);
#2720=ORIENTED_EDGE('',*,*,#2063,.F.);
#2721=ORIENTED_EDGE('',*,*,#2068,.F.);
#2722=ORIENTED_EDGE('',*,*,#2064,.F.);
#2723=ORIENTED_EDGE('',*,*,#2067,.T.);
#2724=ORIENTED_EDGE('',*,*,#2059,.F.);
#2725=ORIENTED_EDGE('',*,*,#2065,.T.);
#2726=ORIENTED_EDGE('',*,*,#2068,.T.);
#2727=ORIENTED_EDGE('',*,*,#2058,.T.);
#2728=ORIENTED_EDGE('',*,*,#2069,.F.);
#2729=ORIENTED_EDGE('',*,*,#2070,.F.);
#2730=ORIENTED_EDGE('',*,*,#2071,.T.);
#2731=ORIENTED_EDGE('',*,*,#2072,.T.);
#2732=ORIENTED_EDGE('',*,*,#2073,.F.);
#2733=ORIENTED_EDGE('',*,*,#2074,.T.);
#2734=ORIENTED_EDGE('',*,*,#2075,.T.);
#2735=ORIENTED_EDGE('',*,*,#2076,.T.);
#2736=ORIENTED_EDGE('',*,*,#2077,.F.);
#2737=ORIENTED_EDGE('',*,*,#2078,.F.);
#2738=ORIENTED_EDGE('',*,*,#2079,.T.);
#2739=ORIENTED_EDGE('',*,*,#2080,.F.);
#2740=ORIENTED_EDGE('',*,*,#2081,.F.);
#2741=ORIENTED_EDGE('',*,*,#2081,.T.);
#2742=ORIENTED_EDGE('',*,*,#2082,.T.);
#2743=ORIENTED_EDGE('',*,*,#2083,.F.);
#2744=ORIENTED_EDGE('',*,*,#2076,.F.);
#2745=ORIENTED_EDGE('',*,*,#2084,.T.);
#2746=ORIENTED_EDGE('',*,*,#2085,.T.);
#2747=ORIENTED_EDGE('',*,*,#2048,.T.);
#2748=ORIENTED_EDGE('',*,*,#2080,.T.);
#2749=ORIENTED_EDGE('',*,*,#2086,.F.);
#2750=ORIENTED_EDGE('',*,*,#2087,.F.);
#2751=ORIENTED_EDGE('',*,*,#2082,.F.);
#2752=ORIENTED_EDGE('',*,*,#2088,.T.);
#2753=ORIENTED_EDGE('',*,*,#2089,.T.);
#2754=ORIENTED_EDGE('',*,*,#2074,.F.);
#2755=ORIENTED_EDGE('',*,*,#2090,.F.);
#2756=ORIENTED_EDGE('',*,*,#2086,.T.);
#2757=ORIENTED_EDGE('',*,*,#2079,.F.);
#2758=ORIENTED_EDGE('',*,*,#2046,.T.);
#2759=ORIENTED_EDGE('',*,*,#2078,.T.);
#2760=ORIENTED_EDGE('',*,*,#2085,.F.);
#2761=ORIENTED_EDGE('',*,*,#2091,.F.);
#2762=ORIENTED_EDGE('',*,*,#2088,.F.);
#2763=ORIENTED_EDGE('',*,*,#2075,.F.);
#2764=ORIENTED_EDGE('',*,*,#2089,.F.);
#2765=ORIENTED_EDGE('',*,*,#2091,.T.);
#2766=ORIENTED_EDGE('',*,*,#2084,.F.);
#2767=ORIENTED_EDGE('',*,*,#2092,.T.);
#2768=ORIENTED_EDGE('',*,*,#2070,.T.);
#2769=ORIENTED_EDGE('',*,*,#2093,.F.);
#2770=ORIENTED_EDGE('',*,*,#2094,.F.);
#2771=ORIENTED_EDGE('',*,*,#2095,.T.);
#2772=ORIENTED_EDGE('',*,*,#2094,.T.);
#2773=ORIENTED_EDGE('',*,*,#2096,.F.);
#2774=ORIENTED_EDGE('',*,*,#2097,.F.);
#2775=ORIENTED_EDGE('',*,*,#2098,.T.);
#2776=ORIENTED_EDGE('',*,*,#2097,.T.);
#2777=ORIENTED_EDGE('',*,*,#2099,.F.);
#2778=ORIENTED_EDGE('',*,*,#2072,.F.);
#2779=ORIENTED_EDGE('',*,*,#2066,.T.);
#2780=ORIENTED_EDGE('',*,*,#2077,.T.);
#2781=ORIENTED_EDGE('',*,*,#2083,.T.);
#2782=ORIENTED_EDGE('',*,*,#2087,.T.);
#2783=ORIENTED_EDGE('',*,*,#2090,.T.);
#2784=ORIENTED_EDGE('',*,*,#2073,.T.);
#2785=ORIENTED_EDGE('',*,*,#2099,.T.);
#2786=ORIENTED_EDGE('',*,*,#2096,.T.);
#2787=ORIENTED_EDGE('',*,*,#2093,.T.);
#2788=ORIENTED_EDGE('',*,*,#2069,.T.);
#2789=ORIENTED_EDGE('',*,*,#2057,.T.);
#2790=ORIENTED_EDGE('',*,*,#2062,.T.);
#2791=ORIENTED_EDGE('',*,*,#2042,.T.);
#2792=ORIENTED_EDGE('',*,*,#2045,.T.);
#2793=ORIENTED_EDGE('',*,*,#2071,.F.);
#2794=ORIENTED_EDGE('',*,*,#2092,.F.);
#2795=ORIENTED_EDGE('',*,*,#2095,.F.);
#2796=ORIENTED_EDGE('',*,*,#2098,.F.);
#2797=ORIENTED_EDGE('',*,*,#2040,.T.);
#2798=ORIENTED_EDGE('',*,*,#2043,.T.);
#2799=ORIENTED_EDGE('',*,*,#2100,.F.);
#2800=ORIENTED_EDGE('',*,*,#2101,.T.);
#2801=ORIENTED_EDGE('',*,*,#2102,.F.);
#2802=ORIENTED_EDGE('',*,*,#2103,.F.);
#2803=ORIENTED_EDGE('',*,*,#2104,.F.);
#2804=ORIENTED_EDGE('',*,*,#2101,.F.);
#2805=ORIENTED_EDGE('',*,*,#2105,.F.);
#2806=ORIENTED_EDGE('',*,*,#2106,.F.);
#2807=ORIENTED_EDGE('',*,*,#2107,.T.);
#2808=ORIENTED_EDGE('',*,*,#2108,.F.);
#2809=ORIENTED_EDGE('',*,*,#2107,.F.);
#2810=ORIENTED_EDGE('',*,*,#2109,.F.);
#2811=ORIENTED_EDGE('',*,*,#2110,.F.);
#2812=ORIENTED_EDGE('',*,*,#2111,.F.);
#2813=ORIENTED_EDGE('',*,*,#2112,.T.);
#2814=ORIENTED_EDGE('',*,*,#2113,.F.);
#2815=ORIENTED_EDGE('',*,*,#2112,.F.);
#2816=ORIENTED_EDGE('',*,*,#2114,.F.);
#2817=ORIENTED_EDGE('',*,*,#2115,.F.);
#2818=ORIENTED_EDGE('',*,*,#2116,.T.);
#2819=ORIENTED_EDGE('',*,*,#2117,.F.);
#2820=ORIENTED_EDGE('',*,*,#2118,.F.);
#2821=ORIENTED_EDGE('',*,*,#2119,.F.);
#2822=ORIENTED_EDGE('',*,*,#2116,.F.);
#2823=ORIENTED_EDGE('',*,*,#2109,.T.);
#2824=ORIENTED_EDGE('',*,*,#2106,.T.);
#2825=ORIENTED_EDGE('',*,*,#2120,.T.);
#2826=ORIENTED_EDGE('',*,*,#2121,.F.);
#2827=ORIENTED_EDGE('',*,*,#2122,.T.);
#2828=ORIENTED_EDGE('',*,*,#2102,.T.);
#2829=ORIENTED_EDGE('',*,*,#2104,.T.);
#2830=ORIENTED_EDGE('',*,*,#2123,.T.);
#2831=ORIENTED_EDGE('',*,*,#2124,.T.);
#2832=ORIENTED_EDGE('',*,*,#2125,.T.);
#2833=ORIENTED_EDGE('',*,*,#2117,.T.);
#2834=ORIENTED_EDGE('',*,*,#2119,.T.);
#2835=ORIENTED_EDGE('',*,*,#2126,.F.);
#2836=ORIENTED_EDGE('',*,*,#2127,.F.);
#2837=ORIENTED_EDGE('',*,*,#2128,.T.);
#2838=ORIENTED_EDGE('',*,*,#2129,.T.);
#2839=ORIENTED_EDGE('',*,*,#2130,.F.);
#2840=ORIENTED_EDGE('',*,*,#2131,.F.);
#2841=ORIENTED_EDGE('',*,*,#2132,.F.);
#2842=ORIENTED_EDGE('',*,*,#2114,.T.);
#2843=ORIENTED_EDGE('',*,*,#2111,.T.);
#2844=ORIENTED_EDGE('',*,*,#2133,.T.);
#2845=ORIENTED_EDGE('',*,*,#2134,.F.);
#2846=ORIENTED_EDGE('',*,*,#2135,.F.);
#2847=ORIENTED_EDGE('',*,*,#2136,.F.);
#2848=ORIENTED_EDGE('',*,*,#2137,.T.);
#2849=ORIENTED_EDGE('',*,*,#2138,.T.);
#2850=ORIENTED_EDGE('',*,*,#2139,.T.);
#2851=ORIENTED_EDGE('',*,*,#2140,.F.);
#2852=ORIENTED_EDGE('',*,*,#2141,.F.);
#2853=ORIENTED_EDGE('',*,*,#2142,.F.);
#2854=ORIENTED_EDGE('',*,*,#2143,.T.);
#2855=ORIENTED_EDGE('',*,*,#2144,.F.);
#2856=ORIENTED_EDGE('',*,*,#2145,.T.);
#2857=ORIENTED_EDGE('',*,*,#2146,.F.);
#2858=ORIENTED_EDGE('',*,*,#2147,.F.);
#2859=ORIENTED_EDGE('',*,*,#2148,.F.);
#2860=ORIENTED_EDGE('',*,*,#2147,.T.);
#2861=ORIENTED_EDGE('',*,*,#2149,.F.);
#2862=ORIENTED_EDGE('',*,*,#2141,.T.);
#2863=ORIENTED_EDGE('',*,*,#2150,.F.);
#2864=ORIENTED_EDGE('',*,*,#2151,.F.);
#2865=ORIENTED_EDGE('',*,*,#2115,.T.);
#2866=ORIENTED_EDGE('',*,*,#2152,.F.);
#2867=ORIENTED_EDGE('',*,*,#2153,.F.);
#2868=ORIENTED_EDGE('',*,*,#2154,.F.);
#2869=ORIENTED_EDGE('',*,*,#2151,.T.);
#2870=ORIENTED_EDGE('',*,*,#2118,.T.);
#2871=ORIENTED_EDGE('',*,*,#2132,.T.);
#2872=ORIENTED_EDGE('',*,*,#2153,.T.);
#2873=ORIENTED_EDGE('',*,*,#2126,.T.);
#2874=ORIENTED_EDGE('',*,*,#2155,.F.);
#2875=ORIENTED_EDGE('',*,*,#2150,.T.);
#2876=ORIENTED_EDGE('',*,*,#2105,.T.);
#2877=ORIENTED_EDGE('',*,*,#2122,.F.);
#2878=ORIENTED_EDGE('',*,*,#2156,.F.);
#2879=ORIENTED_EDGE('',*,*,#2157,.T.);
#2880=ORIENTED_EDGE('',*,*,#2142,.T.);
#2881=ORIENTED_EDGE('',*,*,#2149,.T.);
#2882=ORIENTED_EDGE('',*,*,#2146,.T.);
#2883=ORIENTED_EDGE('',*,*,#2158,.T.);
#2884=ORIENTED_EDGE('',*,*,#2159,.T.);
#2885=ORIENTED_EDGE('',*,*,#2155,.T.);
#2886=ORIENTED_EDGE('',*,*,#2160,.F.);
#2887=ORIENTED_EDGE('',*,*,#2120,.F.);
#2888=ORIENTED_EDGE('',*,*,#2152,.T.);
#2889=ORIENTED_EDGE('',*,*,#2159,.F.);
#2890=ORIENTED_EDGE('',*,*,#2161,.T.);
#2891=ORIENTED_EDGE('',*,*,#2127,.T.);
#2892=ORIENTED_EDGE('',*,*,#2162,.F.);
#2893=ORIENTED_EDGE('',*,*,#2129,.F.);
#2894=ORIENTED_EDGE('',*,*,#2163,.T.);
#2895=ORIENTED_EDGE('',*,*,#2156,.T.);
#2896=ORIENTED_EDGE('',*,*,#2164,.F.);
#2897=ORIENTED_EDGE('',*,*,#2160,.T.);
#2898=ORIENTED_EDGE('',*,*,#2154,.T.);
#2899=ORIENTED_EDGE('',*,*,#2131,.T.);
#2900=ORIENTED_EDGE('',*,*,#2130,.T.);
#2901=ORIENTED_EDGE('',*,*,#2165,.F.);
#2902=ORIENTED_EDGE('',*,*,#2164,.T.);
#2903=ORIENTED_EDGE('',*,*,#2166,.F.);
#2904=ORIENTED_EDGE('',*,*,#2162,.T.);
#2905=ORIENTED_EDGE('',*,*,#2121,.T.);
#2906=ORIENTED_EDGE('',*,*,#2165,.T.);
#2907=ORIENTED_EDGE('',*,*,#2166,.T.);
#2908=ORIENTED_EDGE('',*,*,#2108,.T.);
#2909=ORIENTED_EDGE('',*,*,#2103,.T.);
#2910=ORIENTED_EDGE('',*,*,#2125,.F.);
#2911=ORIENTED_EDGE('',*,*,#2167,.F.);
#2912=ORIENTED_EDGE('',*,*,#2168,.T.);
#2913=ORIENTED_EDGE('',*,*,#2169,.F.);
#2914=ORIENTED_EDGE('',*,*,#2170,.T.);
#2915=ORIENTED_EDGE('',*,*,#2144,.T.);
#2916=ORIENTED_EDGE('',*,*,#2148,.T.);
#2917=ORIENTED_EDGE('',*,*,#2140,.T.);
#2918=ORIENTED_EDGE('',*,*,#2171,.T.);
#2919=ORIENTED_EDGE('',*,*,#2172,.T.);
#2920=ORIENTED_EDGE('',*,*,#2123,.F.);
#2921=ORIENTED_EDGE('',*,*,#2173,.T.);
#2922=ORIENTED_EDGE('',*,*,#2174,.T.);
#2923=ORIENTED_EDGE('',*,*,#2113,.T.);
#2924=ORIENTED_EDGE('',*,*,#2168,.F.);
#2925=ORIENTED_EDGE('',*,*,#2174,.F.);
#2926=ORIENTED_EDGE('',*,*,#2175,.F.);
#2927=ORIENTED_EDGE('',*,*,#2173,.F.);
#2928=ORIENTED_EDGE('',*,*,#2176,.F.);
#2929=ORIENTED_EDGE('',*,*,#2177,.T.);
#2930=ORIENTED_EDGE('',*,*,#2110,.T.);
#2931=ORIENTED_EDGE('',*,*,#2139,.F.);
#2932=ORIENTED_EDGE('',*,*,#2177,.F.);
#2933=ORIENTED_EDGE('',*,*,#2133,.F.);
#2934=ORIENTED_EDGE('',*,*,#2175,.T.);
#2935=ORIENTED_EDGE('',*,*,#2138,.F.);
#2936=ORIENTED_EDGE('',*,*,#2178,.T.);
#2937=ORIENTED_EDGE('',*,*,#2169,.T.);
#2938=ORIENTED_EDGE('',*,*,#2179,.F.);
#2939=ORIENTED_EDGE('',*,*,#2172,.F.);
#2940=ORIENTED_EDGE('',*,*,#2180,.T.);
#2941=ORIENTED_EDGE('',*,*,#2136,.T.);
#2942=ORIENTED_EDGE('',*,*,#2181,.F.);
#2943=ORIENTED_EDGE('',*,*,#2134,.T.);
#2944=ORIENTED_EDGE('',*,*,#2176,.T.);
#2945=ORIENTED_EDGE('',*,*,#2167,.T.);
#2946=ORIENTED_EDGE('',*,*,#2170,.F.);
#2947=ORIENTED_EDGE('',*,*,#2178,.F.);
#2948=ORIENTED_EDGE('',*,*,#2137,.F.);
#2949=ORIENTED_EDGE('',*,*,#2180,.F.);
#2950=ORIENTED_EDGE('',*,*,#2171,.F.);
#2951=ORIENTED_EDGE('',*,*,#2143,.F.);
#2952=ORIENTED_EDGE('',*,*,#2157,.F.);
#2953=ORIENTED_EDGE('',*,*,#2163,.F.);
#2954=ORIENTED_EDGE('',*,*,#2128,.F.);
#2955=ORIENTED_EDGE('',*,*,#2161,.F.);
#2956=ORIENTED_EDGE('',*,*,#2158,.F.);
#2957=ORIENTED_EDGE('',*,*,#2145,.F.);
#2958=ORIENTED_EDGE('',*,*,#2182,.F.);
#2959=ORIENTED_EDGE('',*,*,#2183,.F.);
#2960=ORIENTED_EDGE('',*,*,#2100,.T.);
#2961=ORIENTED_EDGE('',*,*,#2135,.T.);
#2962=ORIENTED_EDGE('',*,*,#2182,.T.);
#2963=ORIENTED_EDGE('',*,*,#2179,.T.);
#2964=ORIENTED_EDGE('',*,*,#2183,.T.);
#2965=ORIENTED_EDGE('',*,*,#2181,.T.);
#2966=ORIENTED_EDGE('',*,*,#2124,.F.);
#2967=ORIENTED_EDGE('',*,*,#2184,.F.);
#2968=ORIENTED_EDGE('',*,*,#2185,.T.);
#2969=ORIENTED_EDGE('',*,*,#2186,.T.);
#2970=ORIENTED_EDGE('',*,*,#2185,.F.);
#2971=ORIENTED_EDGE('',*,*,#2187,.F.);
#2972=ORIENTED_EDGE('',*,*,#2188,.T.);
#2973=ORIENTED_EDGE('',*,*,#2189,.T.);
#2974=ORIENTED_EDGE('',*,*,#2188,.F.);
#2975=ORIENTED_EDGE('',*,*,#2187,.T.);
#2976=ORIENTED_EDGE('',*,*,#2184,.T.);
#2977=ORIENTED_EDGE('',*,*,#2189,.F.);
#2978=ORIENTED_EDGE('',*,*,#2186,.F.);
#2979=ORIENTED_EDGE('',*,*,#2190,.T.);
#2980=ORIENTED_EDGE('',*,*,#2191,.F.);
#2981=ORIENTED_EDGE('',*,*,#2190,.F.);
#2982=ORIENTED_EDGE('',*,*,#2192,.T.);
#2983=ORIENTED_EDGE('',*,*,#2193,.T.);
#2984=ORIENTED_EDGE('',*,*,#2192,.F.);
#2985=ORIENTED_EDGE('',*,*,#2193,.F.);
#2986=ORIENTED_EDGE('',*,*,#2194,.F.);
#2987=ORIENTED_EDGE('',*,*,#2195,.T.);
#2988=ORIENTED_EDGE('',*,*,#2196,.F.);
#2989=ORIENTED_EDGE('',*,*,#2195,.F.);
#2990=ORIENTED_EDGE('',*,*,#2191,.T.);
#2991=ORIENTED_EDGE('',*,*,#2197,.T.);
#2992=ORIENTED_EDGE('',*,*,#2194,.T.);
#2993=ORIENTED_EDGE('',*,*,#2197,.F.);
#2994=ORIENTED_EDGE('',*,*,#2198,.F.);
#2995=ORIENTED_EDGE('',*,*,#2199,.T.);
#2996=ORIENTED_EDGE('',*,*,#2200,.F.);
#2997=ORIENTED_EDGE('',*,*,#2201,.F.);
#2998=ORIENTED_EDGE('',*,*,#2202,.F.);
#2999=ORIENTED_EDGE('',*,*,#2203,.F.);
#3000=ORIENTED_EDGE('',*,*,#2204,.F.);
#3001=ORIENTED_EDGE('',*,*,#2205,.F.);
#3002=ORIENTED_EDGE('',*,*,#2199,.F.);
#3003=ORIENTED_EDGE('',*,*,#2204,.T.);
#3004=ORIENTED_EDGE('',*,*,#2206,.F.);
#3005=ORIENTED_EDGE('',*,*,#2207,.T.);
#3006=ORIENTED_EDGE('',*,*,#2208,.T.);
#3007=ORIENTED_EDGE('',*,*,#2203,.T.);
#3008=ORIENTED_EDGE('',*,*,#2209,.F.);
#3009=ORIENTED_EDGE('',*,*,#2210,.T.);
#3010=ORIENTED_EDGE('',*,*,#2206,.T.);
#3011=ORIENTED_EDGE('',*,*,#2202,.T.);
#3012=ORIENTED_EDGE('',*,*,#2211,.F.);
#3013=ORIENTED_EDGE('',*,*,#2212,.T.);
#3014=ORIENTED_EDGE('',*,*,#2209,.T.);
#3015=ORIENTED_EDGE('',*,*,#2201,.T.);
#3016=ORIENTED_EDGE('',*,*,#2213,.F.);
#3017=ORIENTED_EDGE('',*,*,#2214,.T.);
#3018=ORIENTED_EDGE('',*,*,#2211,.T.);
#3019=ORIENTED_EDGE('',*,*,#2200,.T.);
#3020=ORIENTED_EDGE('',*,*,#2215,.F.);
#3021=ORIENTED_EDGE('',*,*,#2216,.T.);
#3022=ORIENTED_EDGE('',*,*,#2213,.T.);
#3023=ORIENTED_EDGE('',*,*,#2205,.T.);
#3024=ORIENTED_EDGE('',*,*,#2208,.F.);
#3025=ORIENTED_EDGE('',*,*,#2217,.T.);
#3026=ORIENTED_EDGE('',*,*,#2215,.T.);
#3027=ORIENTED_EDGE('',*,*,#2198,.T.);
#3028=ORIENTED_EDGE('',*,*,#2212,.F.);
#3029=ORIENTED_EDGE('',*,*,#2214,.F.);
#3030=ORIENTED_EDGE('',*,*,#2216,.F.);
#3031=ORIENTED_EDGE('',*,*,#2217,.F.);
#3032=ORIENTED_EDGE('',*,*,#2207,.F.);
#3033=ORIENTED_EDGE('',*,*,#2210,.F.);
#3034=ORIENTED_EDGE('',*,*,#2196,.T.);
#3035=ORIENTED_EDGE('',*,*,#2218,.F.);
#3036=ORIENTED_EDGE('',*,*,#2219,.T.);
#3037=ORIENTED_EDGE('',*,*,#2220,.T.);
#3038=ORIENTED_EDGE('',*,*,#2219,.F.);
#3039=ORIENTED_EDGE('',*,*,#2221,.F.);
#3040=ORIENTED_EDGE('',*,*,#2222,.T.);
#3041=ORIENTED_EDGE('',*,*,#2223,.T.);
#3042=ORIENTED_EDGE('',*,*,#2222,.F.);
#3043=ORIENTED_EDGE('',*,*,#2221,.T.);
#3044=ORIENTED_EDGE('',*,*,#2218,.T.);
#3045=ORIENTED_EDGE('',*,*,#2223,.F.);
#3046=ORIENTED_EDGE('',*,*,#2220,.F.);
#3047=ORIENTED_EDGE('',*,*,#2224,.F.);
#3048=ORIENTED_EDGE('',*,*,#2225,.F.);
#3049=ORIENTED_EDGE('',*,*,#2226,.T.);
#3050=ORIENTED_EDGE('',*,*,#2227,.F.);
#3051=ORIENTED_EDGE('',*,*,#2226,.F.);
#3052=ORIENTED_EDGE('',*,*,#2228,.F.);
#3053=ORIENTED_EDGE('',*,*,#2229,.F.);
#3054=ORIENTED_EDGE('',*,*,#2230,.F.);
#3055=ORIENTED_EDGE('',*,*,#2231,.F.);
#3056=ORIENTED_EDGE('',*,*,#2232,.F.);
#3057=ORIENTED_EDGE('',*,*,#2233,.T.);
#3058=ORIENTED_EDGE('',*,*,#2234,.F.);
#3059=ORIENTED_EDGE('',*,*,#2235,.F.);
#3060=ORIENTED_EDGE('',*,*,#2236,.F.);
#3061=ORIENTED_EDGE('',*,*,#2237,.F.);
#3062=ORIENTED_EDGE('',*,*,#2238,.F.);
#3063=ORIENTED_EDGE('',*,*,#2239,.F.);
#3064=ORIENTED_EDGE('',*,*,#2233,.F.);
#3065=ORIENTED_EDGE('',*,*,#2229,.T.);
#3066=ORIENTED_EDGE('',*,*,#2240,.T.);
#3067=ORIENTED_EDGE('',*,*,#2238,.T.);
#3068=ORIENTED_EDGE('',*,*,#2241,.F.);
#3069=ORIENTED_EDGE('',*,*,#2228,.T.);
#3070=ORIENTED_EDGE('',*,*,#2242,.T.);
#3071=ORIENTED_EDGE('',*,*,#2239,.T.);
#3072=ORIENTED_EDGE('',*,*,#2240,.F.);
#3073=ORIENTED_EDGE('',*,*,#2225,.T.);
#3074=ORIENTED_EDGE('',*,*,#2243,.T.);
#3075=ORIENTED_EDGE('',*,*,#2234,.T.);
#3076=ORIENTED_EDGE('',*,*,#2242,.F.);
#3077=ORIENTED_EDGE('',*,*,#2244,.F.);
#3078=ORIENTED_EDGE('',*,*,#2245,.T.);
#3079=ORIENTED_EDGE('',*,*,#2246,.T.);
#3080=ORIENTED_EDGE('',*,*,#2245,.F.);
#3081=ORIENTED_EDGE('',*,*,#2224,.T.);
#3082=ORIENTED_EDGE('',*,*,#2247,.T.);
#3083=ORIENTED_EDGE('',*,*,#2235,.T.);
#3084=ORIENTED_EDGE('',*,*,#2243,.F.);
#3085=ORIENTED_EDGE('',*,*,#2230,.T.);
#3086=ORIENTED_EDGE('',*,*,#2241,.T.);
#3087=ORIENTED_EDGE('',*,*,#2237,.T.);
#3088=ORIENTED_EDGE('',*,*,#2248,.F.);
#3089=ORIENTED_EDGE('',*,*,#2231,.T.);
#3090=ORIENTED_EDGE('',*,*,#2248,.T.);
#3091=ORIENTED_EDGE('',*,*,#2236,.T.);
#3092=ORIENTED_EDGE('',*,*,#2247,.F.);
#3093=ORIENTED_EDGE('',*,*,#2232,.T.);
#3094=ORIENTED_EDGE('',*,*,#2244,.T.);
#3095=ORIENTED_EDGE('',*,*,#2227,.T.);
#3096=ORIENTED_EDGE('',*,*,#2246,.F.);
#3097=CYLINDRICAL_SURFACE('',#3425,0.275);
#3098=CYLINDRICAL_SURFACE('',#3428,0.275);
#3099=CYLINDRICAL_SURFACE('',#3431,0.41);
#3100=CYLINDRICAL_SURFACE('',#3434,0.41);
#3101=CYLINDRICAL_SURFACE('',#3437,0.7);
#3102=CYLINDRICAL_SURFACE('',#3446,0.7);
#3103=CYLINDRICAL_SURFACE('',#3461,0.410000000000047);
#3104=CYLINDRICAL_SURFACE('',#3466,0.410000000000047);
#3105=CYLINDRICAL_SURFACE('',#3471,0.410000000000047);
#3106=CYLINDRICAL_SURFACE('',#3476,0.410000000000047);
#3107=CYLINDRICAL_SURFACE('',#3495,0.70000000000008);
#3108=CYLINDRICAL_SURFACE('',#3498,0.70000000000008);
#3109=CYLINDRICAL_SURFACE('',#3504,0.70000000000008);
#3110=CYLINDRICAL_SURFACE('',#3506,0.70000000000008);
#3111=CYLINDRICAL_SURFACE('',#3514,0.70000000000008);
#3112=CYLINDRICAL_SURFACE('',#3515,0.70000000000008);
#3113=CYLINDRICAL_SURFACE('',#3525,0.70000000000008);
#3114=CYLINDRICAL_SURFACE('',#3526,0.70000000000008);
#3115=CYLINDRICAL_SURFACE('',#3528,0.310000000000035);
#3116=CYLINDRICAL_SURFACE('',#3531,0.400000000000046);
#3117=CYLINDRICAL_SURFACE('',#3540,0.300000000000034);
#3118=CYLINDRICAL_SURFACE('',#3543,0.294200000000034);
#3119=CYLINDRICAL_SURFACE('',#3558,0.320000000000037);
#3120=CYLINDRICAL_SURFACE('',#3561,0.600000000000069);
#3121=CYLINDRICAL_SURFACE('',#3567,0.320000000000037);
#3122=CYLINDRICAL_SURFACE('',#3570,0.600000000000069);
#3123=CYLINDRICAL_SURFACE('',#3583,0.251750000000029);
#3124=CYLINDRICAL_SURFACE('',#3604,0.274999999999999);
#3125=CYLINDRICAL_SURFACE('',#3607,0.274999999999999);
#3126=CYLINDRICAL_SURFACE('',#3610,0.41);
#3127=CYLINDRICAL_SURFACE('',#3613,0.41);
#3128=CYLINDRICAL_SURFACE('',#3616,0.699999999999999);
#3129=CYLINDRICAL_SURFACE('',#3625,0.699999999999999);
#3130=CYLINDRICAL_SURFACE('',#3641,0.41);
#3131=CYLINDRICAL_SURFACE('',#3646,0.41);
#3132=CYLINDRICAL_SURFACE('',#3651,0.41);
#3133=CYLINDRICAL_SURFACE('',#3656,0.41);
#3134=CYLINDRICAL_SURFACE('',#3675,0.7);
#3135=CYLINDRICAL_SURFACE('',#3678,0.7);
#3136=CYLINDRICAL_SURFACE('',#3684,0.7);
#3137=CYLINDRICAL_SURFACE('',#3686,0.7);
#3138=CYLINDRICAL_SURFACE('',#3694,0.7);
#3139=CYLINDRICAL_SURFACE('',#3695,0.7);
#3140=CYLINDRICAL_SURFACE('',#3705,0.7);
#3141=CYLINDRICAL_SURFACE('',#3706,0.7);
#3142=CYLINDRICAL_SURFACE('',#3708,0.31);
#3143=CYLINDRICAL_SURFACE('',#3711,0.4);
#3144=CYLINDRICAL_SURFACE('',#3720,0.3);
#3145=CYLINDRICAL_SURFACE('',#3723,0.2942);
#3146=CYLINDRICAL_SURFACE('',#3738,0.32);
#3147=CYLINDRICAL_SURFACE('',#3741,0.6);
#3148=CYLINDRICAL_SURFACE('',#3754,0.25175);
#3149=ADVANCED_FACE('',(#527),#3097,.F.);
#3150=ADVANCED_FACE('',(#528),#3098,.F.);
#3151=ADVANCED_FACE('',(#529),#3099,.F.);
#3152=ADVANCED_FACE('',(#530),#3100,.F.);
#3153=ADVANCED_FACE('',(#531),#3101,.T.);
#3154=ADVANCED_FACE('',(#532,#363),#405,.T.);
#3155=ADVANCED_FACE('',(#533),#406,.T.);
#3156=ADVANCED_FACE('',(#534,#364),#407,.F.);
#3157=ADVANCED_FACE('',(#535),#408,.T.);
#3158=ADVANCED_FACE('',(#536),#409,.T.);
#3159=ADVANCED_FACE('',(#537,#365,#366),#410,.T.);
#3160=ADVANCED_FACE('',(#538),#3102,.T.);
#3161=ADVANCED_FACE('',(#539,#367),#411,.T.);
#3162=ADVANCED_FACE('',(#540),#412,.T.);
#3163=ADVANCED_FACE('',(#541,#368),#413,.F.);
#3164=ADVANCED_FACE('',(#542),#414,.T.);
#3165=ADVANCED_FACE('',(#543),#415,.T.);
#3166=ADVANCED_FACE('',(#544),#416,.T.);
#3167=ADVANCED_FACE('',(#545),#417,.T.);
#3168=ADVANCED_FACE('',(#546),#418,.T.);
#3169=ADVANCED_FACE('',(#547),#419,.T.);
#3170=ADVANCED_FACE('',(#548,#369,#370),#420,.F.);
#3171=ADVANCED_FACE('',(#549),#3103,.F.);
#3172=ADVANCED_FACE('',(#550),#3104,.F.);
#3173=ADVANCED_FACE('',(#551),#3105,.F.);
#3174=ADVANCED_FACE('',(#552),#3106,.F.);
#3175=ADVANCED_FACE('',(#553),#421,.F.);
#3176=ADVANCED_FACE('',(#554),#422,.T.);
#3177=ADVANCED_FACE('',(#555),#423,.T.);
#3178=ADVANCED_FACE('',(#556),#424,.T.);
#3179=ADVANCED_FACE('',(#557),#425,.T.);
#3180=ADVANCED_FACE('',(#558),#426,.T.);
#3181=ADVANCED_FACE('',(#559),#427,.T.);
#3182=ADVANCED_FACE('',(#560,#371),#428,.F.);
#3183=ADVANCED_FACE('',(#561),#3107,.T.);
#3184=ADVANCED_FACE('',(#562),#429,.T.);
#3185=ADVANCED_FACE('',(#563),#3108,.T.);
#3186=ADVANCED_FACE('',(#564),#430,.T.);
#3187=ADVANCED_FACE('',(#565),#431,.T.);
#3188=ADVANCED_FACE('',(#566),#432,.T.);
#3189=ADVANCED_FACE('',(#567),#433,.T.);
#3190=ADVANCED_FACE('',(#568),#3109,.T.);
#3191=ADVANCED_FACE('',(#569),#3110,.T.);
#3192=ADVANCED_FACE('',(#570,#372),#434,.T.);
#3193=ADVANCED_FACE('',(#571),#435,.T.);
#3194=ADVANCED_FACE('',(#572,#373),#436,.T.);
#3195=ADVANCED_FACE('',(#573),#3111,.T.);
#3196=ADVANCED_FACE('',(#574),#3112,.T.);
#3197=ADVANCED_FACE('',(#575),#437,.F.);
#3198=ADVANCED_FACE('',(#576),#438,.T.);
#3199=ADVANCED_FACE('',(#577),#439,.T.);
#3200=ADVANCED_FACE('',(#578),#440,.T.);
#3201=ADVANCED_FACE('',(#579),#441,.F.);
#3202=ADVANCED_FACE('',(#580,#374),#442,.F.);
#3203=ADVANCED_FACE('',(#581),#3113,.T.);
#3204=ADVANCED_FACE('',(#582),#3114,.T.);
#3205=ADVANCED_FACE('',(#583),#3115,.F.);
#3206=ADVANCED_FACE('',(#584),#3116,.T.);
#3207=ADVANCED_FACE('',(#585,#375),#443,.T.);
#3208=ADVANCED_FACE('',(#586,#376),#444,.F.);
#3209=ADVANCED_FACE('',(#587,#377),#445,.T.);
#3210=ADVANCED_FACE('',(#588),#3117,.T.);
#3211=ADVANCED_FACE('',(#589),#446,.F.);
#3212=ADVANCED_FACE('',(#590),#3118,.T.);
#3213=ADVANCED_FACE('',(#591),#283,.T.);
#3214=ADVANCED_FACE('',(#592),#284,.T.);
#3215=ADVANCED_FACE('',(#593),#447,.T.);
#3216=ADVANCED_FACE('',(#594),#448,.T.);
#3217=ADVANCED_FACE('',(#595),#449,.T.);
#3218=ADVANCED_FACE('',(#596),#450,.T.);
#3219=ADVANCED_FACE('',(#597),#451,.T.);
#3220=ADVANCED_FACE('',(#598),#452,.T.);
#3221=ADVANCED_FACE('',(#599),#453,.T.);
#3222=ADVANCED_FACE('',(#600,#378),#454,.F.);
#3223=ADVANCED_FACE('',(#601),#3119,.F.);
#3224=ADVANCED_FACE('',(#602),#3120,.T.);
#3225=ADVANCED_FACE('',(#603,#379),#455,.T.);
#3226=ADVANCED_FACE('',(#604,#380),#456,.F.);
#3227=ADVANCED_FACE('',(#605),#3121,.F.);
#3228=ADVANCED_FACE('',(#606),#3122,.T.);
#3229=ADVANCED_FACE('',(#607,#381),#457,.T.);
#3230=ADVANCED_FACE('',(#608,#382),#458,.F.);
#3231=ADVANCED_FACE('',(#609),#285,.T.);
#3232=ADVANCED_FACE('',(#610),#286,.T.);
#3233=ADVANCED_FACE('',(#611),#459,.T.);
#3234=ADVANCED_FACE('',(#612),#460,.T.);
#3235=ADVANCED_FACE('',(#613),#461,.T.);
#3236=ADVANCED_FACE('',(#614),#3123,.F.);
#3237=ADVANCED_FACE('',(#615),#462,.T.);
#3238=ADVANCED_FACE('',(#616),#463,.T.);
#3239=ADVANCED_FACE('',(#617),#464,.T.);
#3240=ADVANCED_FACE('',(#618,#383),#465,.T.);
#3241=ADVANCED_FACE('',(#619,#384),#466,.F.);
#3242=ADVANCED_FACE('',(#620),#3124,.F.);
#3243=ADVANCED_FACE('',(#621),#3125,.F.);
#3244=ADVANCED_FACE('',(#622),#3126,.F.);
#3245=ADVANCED_FACE('',(#623),#3127,.F.);
#3246=ADVANCED_FACE('',(#624),#3128,.T.);
#3247=ADVANCED_FACE('',(#625,#385),#467,.T.);
#3248=ADVANCED_FACE('',(#626),#468,.T.);
#3249=ADVANCED_FACE('',(#627,#386),#469,.F.);
#3250=ADVANCED_FACE('',(#628),#470,.T.);
#3251=ADVANCED_FACE('',(#629),#471,.T.);
#3252=ADVANCED_FACE('',(#630),#472,.T.);
#3253=ADVANCED_FACE('',(#631),#3129,.T.);
#3254=ADVANCED_FACE('',(#632,#387),#473,.T.);
#3255=ADVANCED_FACE('',(#633),#474,.T.);
#3256=ADVANCED_FACE('',(#634,#388),#475,.F.);
#3257=ADVANCED_FACE('',(#635),#476,.T.);
#3258=ADVANCED_FACE('',(#636),#477,.T.);
#3259=ADVANCED_FACE('',(#637),#478,.T.);
#3260=ADVANCED_FACE('',(#638),#479,.T.);
#3261=ADVANCED_FACE('',(#639),#480,.T.);
#3262=ADVANCED_FACE('',(#640,#389,#390),#481,.T.);
#3263=ADVANCED_FACE('',(#641,#391,#392),#482,.F.);
#3264=ADVANCED_FACE('',(#642),#3130,.F.);
#3265=ADVANCED_FACE('',(#643),#3131,.F.);
#3266=ADVANCED_FACE('',(#644),#3132,.F.);
#3267=ADVANCED_FACE('',(#645),#3133,.F.);
#3268=ADVANCED_FACE('',(#646),#483,.F.);
#3269=ADVANCED_FACE('',(#647),#484,.T.);
#3270=ADVANCED_FACE('',(#648),#485,.T.);
#3271=ADVANCED_FACE('',(#649),#486,.T.);
#3272=ADVANCED_FACE('',(#650),#487,.T.);
#3273=ADVANCED_FACE('',(#651),#488,.T.);
#3274=ADVANCED_FACE('',(#652),#489,.T.);
#3275=ADVANCED_FACE('',(#653,#393),#490,.F.);
#3276=ADVANCED_FACE('',(#654),#3134,.T.);
#3277=ADVANCED_FACE('',(#655),#491,.T.);
#3278=ADVANCED_FACE('',(#656),#3135,.T.);
#3279=ADVANCED_FACE('',(#657),#492,.T.);
#3280=ADVANCED_FACE('',(#658),#493,.T.);
#3281=ADVANCED_FACE('',(#659),#494,.T.);
#3282=ADVANCED_FACE('',(#660),#495,.T.);
#3283=ADVANCED_FACE('',(#661),#3136,.T.);
#3284=ADVANCED_FACE('',(#662),#3137,.T.);
#3285=ADVANCED_FACE('',(#663,#394),#496,.T.);
#3286=ADVANCED_FACE('',(#664),#497,.T.);
#3287=ADVANCED_FACE('',(#665,#395),#498,.T.);
#3288=ADVANCED_FACE('',(#666),#3138,.T.);
#3289=ADVANCED_FACE('',(#667),#3139,.T.);
#3290=ADVANCED_FACE('',(#668),#499,.F.);
#3291=ADVANCED_FACE('',(#669),#500,.T.);
#3292=ADVANCED_FACE('',(#670),#501,.T.);
#3293=ADVANCED_FACE('',(#671),#502,.T.);
#3294=ADVANCED_FACE('',(#672),#503,.F.);
#3295=ADVANCED_FACE('',(#673,#396),#504,.F.);
#3296=ADVANCED_FACE('',(#674),#3140,.T.);
#3297=ADVANCED_FACE('',(#675),#3141,.T.);
#3298=ADVANCED_FACE('',(#676),#3142,.F.);
#3299=ADVANCED_FACE('',(#677),#3143,.T.);
#3300=ADVANCED_FACE('',(#678,#397),#505,.T.);
#3301=ADVANCED_FACE('',(#679,#398),#506,.F.);
#3302=ADVANCED_FACE('',(#680,#399),#507,.T.);
#3303=ADVANCED_FACE('',(#681),#3144,.T.);
#3304=ADVANCED_FACE('',(#682),#508,.F.);
#3305=ADVANCED_FACE('',(#683),#3145,.T.);
#3306=ADVANCED_FACE('',(#684),#287,.T.);
#3307=ADVANCED_FACE('',(#685),#288,.T.);
#3308=ADVANCED_FACE('',(#686),#509,.T.);
#3309=ADVANCED_FACE('',(#687),#510,.T.);
#3310=ADVANCED_FACE('',(#688),#511,.T.);
#3311=ADVANCED_FACE('',(#689),#512,.T.);
#3312=ADVANCED_FACE('',(#690),#513,.T.);
#3313=ADVANCED_FACE('',(#691),#514,.T.);
#3314=ADVANCED_FACE('',(#692),#515,.T.);
#3315=ADVANCED_FACE('',(#693,#400),#516,.F.);
#3316=ADVANCED_FACE('',(#694),#3146,.F.);
#3317=ADVANCED_FACE('',(#695),#3147,.T.);
#3318=ADVANCED_FACE('',(#696,#401),#517,.T.);
#3319=ADVANCED_FACE('',(#697,#402),#518,.F.);
#3320=ADVANCED_FACE('',(#698),#289,.T.);
#3321=ADVANCED_FACE('',(#699),#290,.T.);
#3322=ADVANCED_FACE('',(#700),#519,.T.);
#3323=ADVANCED_FACE('',(#701),#520,.T.);
#3324=ADVANCED_FACE('',(#702),#521,.T.);
#3325=ADVANCED_FACE('',(#703),#3148,.F.);
#3326=ADVANCED_FACE('',(#704),#522,.T.);
#3327=ADVANCED_FACE('',(#705),#523,.T.);
#3328=ADVANCED_FACE('',(#706),#524,.T.);
#3329=ADVANCED_FACE('',(#707,#403),#525,.T.);
#3330=ADVANCED_FACE('',(#708,#404),#526,.F.);
#3331=CLOSED_SHELL('',(#3149,#3150,#3151,#3152,#3153,#3154,#3155,#3156,
#3157,#3158,#3159,#3160,#3161,#3162,#3163,#3164,#3165,#3166,#3167,#3168,
#3169,#3170));
#3332=CLOSED_SHELL('',(#3171,#3172,#3173,#3174,#3175,#3176,#3177,#3178,
#3179,#3180,#3181,#3182,#3183,#3184,#3185,#3186,#3187,#3188,#3189,#3190,
#3191,#3192,#3193,#3194,#3195,#3196,#3197,#3198,#3199,#3200,#3201,#3202,
#3203,#3204));
#3333=CLOSED_SHELL('',(#3205,#3206,#3207,#3208));
#3334=CLOSED_SHELL('',(#3209,#3210,#3211,#3212,#3213,#3214,#3215,#3216,
#3217,#3218,#3219,#3220,#3221,#3222));
#3335=CLOSED_SHELL('',(#3223,#3224,#3225,#3226));
#3336=CLOSED_SHELL('',(#3227,#3228,#3229,#3230));
#3337=CLOSED_SHELL('',(#3231,#3232,#3233,#3234,#3235,#3236,#3237,#3238,
#3239,#3240,#3241));
#3338=CLOSED_SHELL('',(#3242,#3243,#3244,#3245,#3246,#3247,#3248,#3249,
#3250,#3251,#3252,#3253,#3254,#3255,#3256,#3257,#3258,#3259,#3260,#3261,
#3262,#3263));
#3339=CLOSED_SHELL('',(#3264,#3265,#3266,#3267,#3268,#3269,#3270,#3271,
#3272,#3273,#3274,#3275,#3276,#3277,#3278,#3279,#3280,#3281,#3282,#3283,
#3284,#3285,#3286,#3287,#3288,#3289,#3290,#3291,#3292,#3293,#3294,#3295,
#3296,#3297));
#3340=CLOSED_SHELL('',(#3298,#3299,#3300,#3301));
#3341=CLOSED_SHELL('',(#3302,#3303,#3304,#3305,#3306,#3307,#3308,#3309,
#3310,#3311,#3312,#3313,#3314,#3315));
#3342=CLOSED_SHELL('',(#3316,#3317,#3318,#3319));
#3343=CLOSED_SHELL('',(#3320,#3321,#3322,#3323,#3324,#3325,#3326,#3327,
#3328,#3329,#3330));
#3344=DERIVED_UNIT_ELEMENT(#3358,1.);
#3345=DERIVED_UNIT_ELEMENT(#5931,-3.);
#3346=DERIVED_UNIT_ELEMENT(#3358,1.);
#3347=DERIVED_UNIT_ELEMENT(#5931,-3.);
#3348=DERIVED_UNIT_ELEMENT(#3358,1.);
#3349=DERIVED_UNIT_ELEMENT(#5931,-3.);
#3350=DERIVED_UNIT_ELEMENT(#3358,1.);
#3351=DERIVED_UNIT_ELEMENT(#5931,-3.);
#3352=DERIVED_UNIT_ELEMENT(#3358,1.);
#3353=DERIVED_UNIT_ELEMENT(#5931,-3.);
#3354=DERIVED_UNIT_ELEMENT(#3358,1.);
#3355=DERIVED_UNIT_ELEMENT(#5931,-3.);
#3356=DERIVED_UNIT_ELEMENT(#3358,1.);
#3357=DERIVED_UNIT_ELEMENT(#5931,-3.);
#3358=(
MASS_UNIT()
NAMED_UNIT(*)
SI_UNIT(.KILO.,.GRAM.)
);
#3359=DERIVED_UNIT((#3344,#3345));
#3360=DERIVED_UNIT((#3346,#3347));
#3361=DERIVED_UNIT((#3348,#3349));
#3362=DERIVED_UNIT((#3350,#3351));
#3363=DERIVED_UNIT((#3352,#3353));
#3364=DERIVED_UNIT((#3354,#3355));
#3365=DERIVED_UNIT((#3356,#3357));
#3366=MEASURE_REPRESENTATION_ITEM('density measure',
POSITIVE_RATIO_MEASURE(7850.),#3359);
#3367=MEASURE_REPRESENTATION_ITEM('density measure',
POSITIVE_RATIO_MEASURE(7850.),#3360);
#3368=MEASURE_REPRESENTATION_ITEM('density measure',
POSITIVE_RATIO_MEASURE(7850.),#3361);
#3369=MEASURE_REPRESENTATION_ITEM('density measure',
POSITIVE_RATIO_MEASURE(7850.),#3362);
#3370=MEASURE_REPRESENTATION_ITEM('density measure',
POSITIVE_RATIO_MEASURE(7850.),#3363);
#3371=MEASURE_REPRESENTATION_ITEM('density measure',
POSITIVE_RATIO_MEASURE(7850.),#3364);
#3372=MEASURE_REPRESENTATION_ITEM('density measure',
POSITIVE_RATIO_MEASURE(7850.),#3365);
#3373=PROPERTY_DEFINITION_REPRESENTATION(#3408,#3387);
#3374=PROPERTY_DEFINITION_REPRESENTATION(#3409,#3388);
#3375=PROPERTY_DEFINITION_REPRESENTATION(#3410,#3389);
#3376=PROPERTY_DEFINITION_REPRESENTATION(#3411,#3390);
#3377=PROPERTY_DEFINITION_REPRESENTATION(#3412,#3391);
#3378=PROPERTY_DEFINITION_REPRESENTATION(#3413,#3392);
#3379=PROPERTY_DEFINITION_REPRESENTATION(#3414,#3393);
#3380=PROPERTY_DEFINITION_REPRESENTATION(#3415,#3394);
#3381=PROPERTY_DEFINITION_REPRESENTATION(#3416,#3395);
#3382=PROPERTY_DEFINITION_REPRESENTATION(#3417,#3396);
#3383=PROPERTY_DEFINITION_REPRESENTATION(#3418,#3397);
#3384=PROPERTY_DEFINITION_REPRESENTATION(#3419,#3398);
#3385=PROPERTY_DEFINITION_REPRESENTATION(#3420,#3399);
#3386=PROPERTY_DEFINITION_REPRESENTATION(#3421,#3400);
#3387=REPRESENTATION('material name',(#3401),#5908);
#3388=REPRESENTATION('density',(#3366),#5908);
#3389=REPRESENTATION('material name',(#3402),#5910);
#3390=REPRESENTATION('density',(#3367),#5910);
#3391=REPRESENTATION('material name',(#3403),#5911);
#3392=REPRESENTATION('density',(#3368),#5911);
#3393=REPRESENTATION('material name',(#3404),#5912);
#3394=REPRESENTATION('density',(#3369),#5912);
#3395=REPRESENTATION('material name',(#3405),#5914);
#3396=REPRESENTATION('density',(#3370),#5914);
#3397=REPRESENTATION('material name',(#3406),#5915);
#3398=REPRESENTATION('density',(#3371),#5915);
#3399=REPRESENTATION('material name',(#3407),#5922);
#3400=REPRESENTATION('density',(#3372),#5922);
#3401=DESCRIPTIVE_REPRESENTATION_ITEM('Steel','Steel');
#3402=DESCRIPTIVE_REPRESENTATION_ITEM('Steel','Steel');
#3403=DESCRIPTIVE_REPRESENTATION_ITEM('Steel','Steel');
#3404=DESCRIPTIVE_REPRESENTATION_ITEM('Steel','Steel');
#3405=DESCRIPTIVE_REPRESENTATION_ITEM('Steel','Steel');
#3406=DESCRIPTIVE_REPRESENTATION_ITEM('Steel','Steel');
#3407=DESCRIPTIVE_REPRESENTATION_ITEM('Steel','Steel');
#3408=PROPERTY_DEFINITION('material property','material name',#6065);
#3409=PROPERTY_DEFINITION('material property','density of part',#6065);
#3410=PROPERTY_DEFINITION('material property','material name',#6067);
#3411=PROPERTY_DEFINITION('material property','density of part',#6067);
#3412=PROPERTY_DEFINITION('material property','material name',#6068);
#3413=PROPERTY_DEFINITION('material property','density of part',#6068);
#3414=PROPERTY_DEFINITION('material property','material name',#6069);
#3415=PROPERTY_DEFINITION('material property','density of part',#6069);
#3416=PROPERTY_DEFINITION('material property','material name',#6071);
#3417=PROPERTY_DEFINITION('material property','density of part',#6071);
#3418=PROPERTY_DEFINITION('material property','material name',#6072);
#3419=PROPERTY_DEFINITION('material property','density of part',#6072);
#3420=PROPERTY_DEFINITION('material property','material name',#6079);
#3421=PROPERTY_DEFINITION('material property','density of part',#6079);
#3422=AXIS2_PLACEMENT_3D('',#4858,#3814,#3815);
#3423=AXIS2_PLACEMENT_3D('',#4859,#3816,#3817);
#3424=AXIS2_PLACEMENT_3D('',#4860,#3818,#3819);
#3425=AXIS2_PLACEMENT_3D('',#4861,#3820,#3821);
#3426=AXIS2_PLACEMENT_3D('',#4863,#3822,#3823);
#3427=AXIS2_PLACEMENT_3D('',#4866,#3825,#3826);
#3428=AXIS2_PLACEMENT_3D('',#4867,#3827,#3828);
#3429=AXIS2_PLACEMENT_3D('',#4869,#3829,#3830);
#3430=AXIS2_PLACEMENT_3D('',#4872,#3832,#3833);
#3431=AXIS2_PLACEMENT_3D('',#4873,#3834,#3835);
#3432=AXIS2_PLACEMENT_3D('',#4875,#3836,#3837);
#3433=AXIS2_PLACEMENT_3D('',#4878,#3839,#3840);
#3434=AXIS2_PLACEMENT_3D('',#4879,#3841,#3842);
#3435=AXIS2_PLACEMENT_3D('',#4881,#3843,#3844);
#3436=AXIS2_PLACEMENT_3D('',#4884,#3846,#3847);
#3437=AXIS2_PLACEMENT_3D('',#4885,#3848,#3849);
#3438=AXIS2_PLACEMENT_3D('',#4890,#3851,#3852);
#3439=AXIS2_PLACEMENT_3D('',#4893,#3854,#3855);
#3440=AXIS2_PLACEMENT_3D('',#4894,#3856,#3857);
#3441=AXIS2_PLACEMENT_3D('',#4904,#3863,#3864);
#3442=AXIS2_PLACEMENT_3D('',#4908,#3867,#3868);
#3443=AXIS2_PLACEMENT_3D('',#4916,#3873,#3874);
#3444=AXIS2_PLACEMENT_3D('',#4918,#3876,#3877);
#3445=AXIS2_PLACEMENT_3D('',#4920,#3879,#3880);
#3446=AXIS2_PLACEMENT_3D('',#4938,#3890,#3891);
#3447=AXIS2_PLACEMENT_3D('',#4943,#3893,#3894);
#3448=AXIS2_PLACEMENT_3D('',#4946,#3896,#3897);
#3449=AXIS2_PLACEMENT_3D('',#4947,#3898,#3899);
#3450=AXIS2_PLACEMENT_3D('',#4954,#3904,#3905);
#3451=AXIS2_PLACEMENT_3D('',#4958,#3908,#3909);
#3452=AXIS2_PLACEMENT_3D('',#4963,#3913,#3914);
#3453=AXIS2_PLACEMENT_3D('',#4965,#3916,#3917);
#3454=AXIS2_PLACEMENT_3D('',#4966,#3918,#3919);
#3455=AXIS2_PLACEMENT_3D('',#4972,#3923,#3924);
#3456=AXIS2_PLACEMENT_3D('',#4976,#3927,#3928);
#3457=AXIS2_PLACEMENT_3D('',#4980,#3931,#3932);
#3458=AXIS2_PLACEMENT_3D('',#4982,#3934,#3935);
#3459=AXIS2_PLACEMENT_3D('',#4983,#3936,#3937);
#3460=AXIS2_PLACEMENT_3D('',#4984,#3938,#3939);
#3461=AXIS2_PLACEMENT_3D('',#4985,#3940,#3941);
#3462=AXIS2_PLACEMENT_3D('',#4987,#3942,#3943);
#3463=AXIS2_PLACEMENT_3D('',#4991,#3945,#3946);
#3464=AXIS2_PLACEMENT_3D('',#4993,#3947,#3948);
#3465=AXIS2_PLACEMENT_3D('',#4994,#3949,#3950);
#3466=AXIS2_PLACEMENT_3D('',#4995,#3951,#3952);
#3467=AXIS2_PLACEMENT_3D('',#4998,#3953,#3954);
#3468=AXIS2_PLACEMENT_3D('',#5000,#3955,#3956);
#3469=AXIS2_PLACEMENT_3D('',#5003,#3958,#3959);
#3470=AXIS2_PLACEMENT_3D('',#5004,#3960,#3961);
#3471=AXIS2_PLACEMENT_3D('',#5005,#3962,#3963);
#3472=AXIS2_PLACEMENT_3D('',#5008,#3964,#3965);
#3473=AXIS2_PLACEMENT_3D('',#5010,#3966,#3967);
#3474=AXIS2_PLACEMENT_3D('',#5013,#3969,#3970);
#3475=AXIS2_PLACEMENT_3D('',#5014,#3971,#3972);
#3476=AXIS2_PLACEMENT_3D('',#5015,#3973,#3974);
#3477=AXIS2_PLACEMENT_3D('',#5017,#3975,#3976);
#3478=AXIS2_PLACEMENT_3D('',#5021,#3978,#3979);
#3479=AXIS2_PLACEMENT_3D('',#5023,#3980,#3981);
#3480=AXIS2_PLACEMENT_3D('',#5024,#3982,#3983);
#3481=AXIS2_PLACEMENT_3D('',#5025,#3984,#3985);
#3482=AXIS2_PLACEMENT_3D('',#5029,#3987,#3988);
#3483=AXIS2_PLACEMENT_3D('',#5031,#3990,#3991);
#3484=AXIS2_PLACEMENT_3D('',#5035,#3993,#3994);
#3485=AXIS2_PLACEMENT_3D('',#5037,#3996,#3997);
#3486=AXIS2_PLACEMENT_3D('',#5047,#4002,#4003);
#3487=AXIS2_PLACEMENT_3D('',#5051,#4006,#4007);
#3488=AXIS2_PLACEMENT_3D('',#5057,#4010,#4011);
#3489=AXIS2_PLACEMENT_3D('',#5065,#4016,#4017);
#3490=AXIS2_PLACEMENT_3D('',#5074,#4022,#4023);
#3491=AXIS2_PLACEMENT_3D('',#5083,#4028,#4029);
#3492=AXIS2_PLACEMENT_3D('',#5086,#4032,#4033);
#3493=AXIS2_PLACEMENT_3D('',#5089,#4034,#4035);
#3494=AXIS2_PLACEMENT_3D('',#5090,#4036,#4037);
#3495=AXIS2_PLACEMENT_3D('',#5091,#4038,#4039);
#3496=AXIS2_PLACEMENT_3D('',#5093,#4041,#4042);
#3497=AXIS2_PLACEMENT_3D('',#5095,#4044,#4045);
#3498=AXIS2_PLACEMENT_3D('',#5096,#4046,#4047);
#3499=AXIS2_PLACEMENT_3D('',#5097,#4048,#4049);
#3500=AXIS2_PLACEMENT_3D('',#5098,#4050,#4051);
#3501=AXIS2_PLACEMENT_3D('',#5106,#4057,#4058);
#3502=AXIS2_PLACEMENT_3D('',#5108,#4060,#4061);
#3503=AXIS2_PLACEMENT_3D('',#5111,#4064,#4065);
#3504=AXIS2_PLACEMENT_3D('',#5113,#4067,#4068);
#3505=AXIS2_PLACEMENT_3D('',#5114,#4069,#4070);
#3506=AXIS2_PLACEMENT_3D('',#5115,#4071,#4072);
#3507=AXIS2_PLACEMENT_3D('',#5116,#4073,#4074);
#3508=AXIS2_PLACEMENT_3D('',#5117,#4075,#4076);
#3509=AXIS2_PLACEMENT_3D('',#5118,#4077,#4078);
#3510=AXIS2_PLACEMENT_3D('',#5122,#4080,#4081);
#3511=AXIS2_PLACEMENT_3D('',#5129,#4086,#4087);
#3512=AXIS2_PLACEMENT_3D('',#5130,#4088,#4089);
#3513=AXIS2_PLACEMENT_3D('',#5131,#4090,#4091);
#3514=AXIS2_PLACEMENT_3D('',#5132,#4092,#4093);
#3515=AXIS2_PLACEMENT_3D('',#5133,#4094,#4095);
#3516=AXIS2_PLACEMENT_3D('',#5136,#4098,#4099);
#3517=AXIS2_PLACEMENT_3D('',#5137,#4100,#4101);
#3518=AXIS2_PLACEMENT_3D('',#5138,#4102,#4103);
#3519=AXIS2_PLACEMENT_3D('',#5140,#4105,#4106);
#3520=AXIS2_PLACEMENT_3D('',#5143,#4109,#4110);
#3521=AXIS2_PLACEMENT_3D('',#5145,#4112,#4113);
#3522=AXIS2_PLACEMENT_3D('',#5146,#4114,#4115);
#3523=AXIS2_PLACEMENT_3D('',#5147,#4116,#4117);
#3524=AXIS2_PLACEMENT_3D('',#5148,#4118,#4119);
#3525=AXIS2_PLACEMENT_3D('',#5149,#4120,#4121);
#3526=AXIS2_PLACEMENT_3D('',#5150,#4122,#4123);
#3527=AXIS2_PLACEMENT_3D('',#5151,#4124,#4125);
#3528=AXIS2_PLACEMENT_3D('',#5152,#4126,#4127);
#3529=AXIS2_PLACEMENT_3D('',#5154,#4128,#4129);
#3530=AXIS2_PLACEMENT_3D('',#5157,#4131,#4132);
#3531=AXIS2_PLACEMENT_3D('',#5158,#4133,#4134);
#3532=AXIS2_PLACEMENT_3D('',#5160,#4135,#4136);
#3533=AXIS2_PLACEMENT_3D('',#5163,#4138,#4139);
#3534=AXIS2_PLACEMENT_3D('',#5164,#4140,#4141);
#3535=AXIS2_PLACEMENT_3D('',#5165,#4142,#4143);
#3536=AXIS2_PLACEMENT_3D('',#5166,#4144,#4145);
#3537=AXIS2_PLACEMENT_3D('',#5167,#4146,#4147);
#3538=AXIS2_PLACEMENT_3D('',#5169,#4148,#4149);
#3539=AXIS2_PLACEMENT_3D('',#5171,#4150,#4151);
#3540=AXIS2_PLACEMENT_3D('',#5172,#4152,#4153);
#3541=AXIS2_PLACEMENT_3D('',#5175,#4155,#4156);
#3542=AXIS2_PLACEMENT_3D('',#5176,#4157,#4158);
#3543=AXIS2_PLACEMENT_3D('',#5177,#4159,#4160);
#3544=AXIS2_PLACEMENT_3D('',#5179,#4161,#4162);
#3545=AXIS2_PLACEMENT_3D('',#5182,#4164,#4165);
#3546=AXIS2_PLACEMENT_3D('',#5183,#4166,#4167);
#3547=AXIS2_PLACEMENT_3D('',#5185,#4169,#4170);
#3548=AXIS2_PLACEMENT_3D('',#5187,#4171,#4172);
#3549=AXIS2_PLACEMENT_3D('',#5213,#4174,#4175);
#3550=AXIS2_PLACEMENT_3D('',#5219,#4179,#4180);
#3551=AXIS2_PLACEMENT_3D('',#5223,#4183,#4184);
#3552=AXIS2_PLACEMENT_3D('',#5227,#4187,#4188);
#3553=AXIS2_PLACEMENT_3D('',#5231,#4191,#4192);
#3554=AXIS2_PLACEMENT_3D('',#5235,#4195,#4196);
#3555=AXIS2_PLACEMENT_3D('',#5237,#4198,#4199);
#3556=AXIS2_PLACEMENT_3D('',#5238,#4200,#4201);
#3557=AXIS2_PLACEMENT_3D('',#5239,#4202,#4203);
#3558=AXIS2_PLACEMENT_3D('',#5240,#4204,#4205);
#3559=AXIS2_PLACEMENT_3D('',#5242,#4206,#4207);
#3560=AXIS2_PLACEMENT_3D('',#5245,#4209,#4210);
#3561=AXIS2_PLACEMENT_3D('',#5246,#4211,#4212);
#3562=AXIS2_PLACEMENT_3D('',#5248,#4213,#4214);
#3563=AXIS2_PLACEMENT_3D('',#5251,#4216,#4217);
#3564=AXIS2_PLACEMENT_3D('',#5252,#4218,#4219);
#3565=AXIS2_PLACEMENT_3D('',#5253,#4220,#4221);
#3566=AXIS2_PLACEMENT_3D('',#5254,#4222,#4223);
#3567=AXIS2_PLACEMENT_3D('',#5255,#4224,#4225);
#3568=AXIS2_PLACEMENT_3D('',#5257,#4226,#4227);
#3569=AXIS2_PLACEMENT_3D('',#5260,#4229,#4230);
#3570=AXIS2_PLACEMENT_3D('',#5261,#4231,#4232);
#3571=AXIS2_PLACEMENT_3D('',#5263,#4233,#4234);
#3572=AXIS2_PLACEMENT_3D('',#5266,#4236,#4237);
#3573=AXIS2_PLACEMENT_3D('',#5267,#4238,#4239);
#3574=AXIS2_PLACEMENT_3D('',#5268,#4240,#4241);
#3575=AXIS2_PLACEMENT_3D('',#5269,#4242,#4243);
#3576=AXIS2_PLACEMENT_3D('',#5270,#4244,#4245);
#3577=AXIS2_PLACEMENT_3D('',#5282,#4247,#4248);
#3578=AXIS2_PLACEMENT_3D('',#5298,#4249,#4250);
#3579=AXIS2_PLACEMENT_3D('',#5300,#4251,#4252);
#3580=AXIS2_PLACEMENT_3D('',#5326,#4254,#4255);
#3581=AXIS2_PLACEMENT_3D('',#5329,#4258,#4259);
#3582=AXIS2_PLACEMENT_3D('',#5331,#4261,#4262);
#3583=AXIS2_PLACEMENT_3D('',#5333,#4264,#4265);
#3584=AXIS2_PLACEMENT_3D('',#5335,#4266,#4267);
#3585=AXIS2_PLACEMENT_3D('',#5338,#4269,#4270);
#3586=AXIS2_PLACEMENT_3D('',#5339,#4271,#4272);
#3587=AXIS2_PLACEMENT_3D('',#5341,#4274,#4275);
#3588=AXIS2_PLACEMENT_3D('',#5343,#4277,#4278);
#3589=AXIS2_PLACEMENT_3D('',#5344,#4279,#4280);
#3590=AXIS2_PLACEMENT_3D('',#5345,#4281,#4282);
#3591=AXIS2_PLACEMENT_3D('',#5346,#4283,#4284);
#3592=AXIS2_PLACEMENT_3D('',#5347,#4285,#4286);
#3593=AXIS2_PLACEMENT_3D('',#5348,#4287,#4288);
#3594=AXIS2_PLACEMENT_3D('',#5349,#4289,#4290);
#3595=AXIS2_PLACEMENT_3D('',#5350,#4291,#4292);
#3596=AXIS2_PLACEMENT_3D('',#5351,#4293,#4294);
#3597=AXIS2_PLACEMENT_3D('',#5352,#4295,#4296);
#3598=AXIS2_PLACEMENT_3D('',#5353,#4297,#4298);
#3599=AXIS2_PLACEMENT_3D('',#5354,#4299,#4300);
#3600=AXIS2_PLACEMENT_3D('',#5355,#4301,#4302);
#3601=AXIS2_PLACEMENT_3D('',#5356,#4303,#4304);
#3602=AXIS2_PLACEMENT_3D('',#5357,#4305,#4306);
#3603=AXIS2_PLACEMENT_3D('',#5358,#4307,#4308);
#3604=AXIS2_PLACEMENT_3D('',#5359,#4309,#4310);
#3605=AXIS2_PLACEMENT_3D('',#5361,#4311,#4312);
#3606=AXIS2_PLACEMENT_3D('',#5364,#4314,#4315);
#3607=AXIS2_PLACEMENT_3D('',#5365,#4316,#4317);
#3608=AXIS2_PLACEMENT_3D('',#5367,#4318,#4319);
#3609=AXIS2_PLACEMENT_3D('',#5370,#4321,#4322);
#3610=AXIS2_PLACEMENT_3D('',#5371,#4323,#4324);
#3611=AXIS2_PLACEMENT_3D('',#5373,#4325,#4326);
#3612=AXIS2_PLACEMENT_3D('',#5376,#4328,#4329);
#3613=AXIS2_PLACEMENT_3D('',#5377,#4330,#4331);
#3614=AXIS2_PLACEMENT_3D('',#5379,#4332,#4333);
#3615=AXIS2_PLACEMENT_3D('',#5382,#4335,#4336);
#3616=AXIS2_PLACEMENT_3D('',#5383,#4337,#4338);
#3617=AXIS2_PLACEMENT_3D('',#5388,#4340,#4341);
#3618=AXIS2_PLACEMENT_3D('',#5391,#4343,#4344);
#3619=AXIS2_PLACEMENT_3D('',#5392,#4345,#4346);
#3620=AXIS2_PLACEMENT_3D('',#5402,#4352,#4353);
#3621=AXIS2_PLACEMENT_3D('',#5406,#4356,#4357);
#3622=AXIS2_PLACEMENT_3D('',#5414,#4362,#4363);
#3623=AXIS2_PLACEMENT_3D('',#5416,#4365,#4366);
#3624=AXIS2_PLACEMENT_3D('',#5418,#4368,#4369);
#3625=AXIS2_PLACEMENT_3D('',#5436,#4379,#4380);
#3626=AXIS2_PLACEMENT_3D('',#5441,#4382,#4383);
#3627=AXIS2_PLACEMENT_3D('',#5444,#4385,#4386);
#3628=AXIS2_PLACEMENT_3D('',#5445,#4387,#4388);
#3629=AXIS2_PLACEMENT_3D('',#5452,#4393,#4394);
#3630=AXIS2_PLACEMENT_3D('',#5456,#4397,#4398);
#3631=AXIS2_PLACEMENT_3D('',#5461,#4402,#4403);
#3632=AXIS2_PLACEMENT_3D('',#5463,#4405,#4406);
#3633=AXIS2_PLACEMENT_3D('',#5464,#4407,#4408);
#3634=AXIS2_PLACEMENT_3D('',#5470,#4412,#4413);
#3635=AXIS2_PLACEMENT_3D('',#5476,#4417,#4418);
#3636=AXIS2_PLACEMENT_3D('',#5479,#4421,#4422);
#3637=AXIS2_PLACEMENT_3D('',#5480,#4423,#4424);
#3638=AXIS2_PLACEMENT_3D('',#5481,#4425,#4426);
#3639=AXIS2_PLACEMENT_3D('',#5482,#4427,#4428);
#3640=AXIS2_PLACEMENT_3D('',#5483,#4429,#4430);
#3641=AXIS2_PLACEMENT_3D('',#5484,#4431,#4432);
#3642=AXIS2_PLACEMENT_3D('',#5486,#4433,#4434);
#3643=AXIS2_PLACEMENT_3D('',#5490,#4436,#4437);
#3644=AXIS2_PLACEMENT_3D('',#5492,#4438,#4439);
#3645=AXIS2_PLACEMENT_3D('',#5493,#4440,#4441);
#3646=AXIS2_PLACEMENT_3D('',#5494,#4442,#4443);
#3647=AXIS2_PLACEMENT_3D('',#5497,#4444,#4445);
#3648=AXIS2_PLACEMENT_3D('',#5499,#4446,#4447);
#3649=AXIS2_PLACEMENT_3D('',#5502,#4449,#4450);
#3650=AXIS2_PLACEMENT_3D('',#5503,#4451,#4452);
#3651=AXIS2_PLACEMENT_3D('',#5504,#4453,#4454);
#3652=AXIS2_PLACEMENT_3D('',#5507,#4455,#4456);
#3653=AXIS2_PLACEMENT_3D('',#5509,#4457,#4458);
#3654=AXIS2_PLACEMENT_3D('',#5512,#4460,#4461);
#3655=AXIS2_PLACEMENT_3D('',#5513,#4462,#4463);
#3656=AXIS2_PLACEMENT_3D('',#5514,#4464,#4465);
#3657=AXIS2_PLACEMENT_3D('',#5516,#4466,#4467);
#3658=AXIS2_PLACEMENT_3D('',#5520,#4469,#4470);
#3659=AXIS2_PLACEMENT_3D('',#5522,#4471,#4472);
#3660=AXIS2_PLACEMENT_3D('',#5523,#4473,#4474);
#3661=AXIS2_PLACEMENT_3D('',#5524,#4475,#4476);
#3662=AXIS2_PLACEMENT_3D('',#5528,#4478,#4479);
#3663=AXIS2_PLACEMENT_3D('',#5530,#4481,#4482);
#3664=AXIS2_PLACEMENT_3D('',#5534,#4484,#4485);
#3665=AXIS2_PLACEMENT_3D('',#5536,#4487,#4488);
#3666=AXIS2_PLACEMENT_3D('',#5546,#4493,#4494);
#3667=AXIS2_PLACEMENT_3D('',#5550,#4497,#4498);
#3668=AXIS2_PLACEMENT_3D('',#5556,#4501,#4502);
#3669=AXIS2_PLACEMENT_3D('',#5564,#4507,#4508);
#3670=AXIS2_PLACEMENT_3D('',#5573,#4513,#4514);
#3671=AXIS2_PLACEMENT_3D('',#5582,#4519,#4520);
#3672=AXIS2_PLACEMENT_3D('',#5585,#4523,#4524);
#3673=AXIS2_PLACEMENT_3D('',#5588,#4525,#4526);
#3674=AXIS2_PLACEMENT_3D('',#5589,#4527,#4528);
#3675=AXIS2_PLACEMENT_3D('',#5590,#4529,#4530);
#3676=AXIS2_PLACEMENT_3D('',#5592,#4532,#4533);
#3677=AXIS2_PLACEMENT_3D('',#5594,#4535,#4536);
#3678=AXIS2_PLACEMENT_3D('',#5595,#4537,#4538);
#3679=AXIS2_PLACEMENT_3D('',#5596,#4539,#4540);
#3680=AXIS2_PLACEMENT_3D('',#5597,#4541,#4542);
#3681=AXIS2_PLACEMENT_3D('',#5605,#4548,#4549);
#3682=AXIS2_PLACEMENT_3D('',#5607,#4551,#4552);
#3683=AXIS2_PLACEMENT_3D('',#5610,#4555,#4556);
#3684=AXIS2_PLACEMENT_3D('',#5612,#4558,#4559);
#3685=AXIS2_PLACEMENT_3D('',#5613,#4560,#4561);
#3686=AXIS2_PLACEMENT_3D('',#5614,#4562,#4563);
#3687=AXIS2_PLACEMENT_3D('',#5615,#4564,#4565);
#3688=AXIS2_PLACEMENT_3D('',#5616,#4566,#4567);
#3689=AXIS2_PLACEMENT_3D('',#5617,#4568,#4569);
#3690=AXIS2_PLACEMENT_3D('',#5621,#4571,#4572);
#3691=AXIS2_PLACEMENT_3D('',#5628,#4577,#4578);
#3692=AXIS2_PLACEMENT_3D('',#5629,#4579,#4580);
#3693=AXIS2_PLACEMENT_3D('',#5630,#4581,#4582);
#3694=AXIS2_PLACEMENT_3D('',#5631,#4583,#4584);
#3695=AXIS2_PLACEMENT_3D('',#5632,#4585,#4586);
#3696=AXIS2_PLACEMENT_3D('',#5635,#4589,#4590);
#3697=AXIS2_PLACEMENT_3D('',#5636,#4591,#4592);
#3698=AXIS2_PLACEMENT_3D('',#5637,#4593,#4594);
#3699=AXIS2_PLACEMENT_3D('',#5639,#4596,#4597);
#3700=AXIS2_PLACEMENT_3D('',#5642,#4600,#4601);
#3701=AXIS2_PLACEMENT_3D('',#5644,#4603,#4604);
#3702=AXIS2_PLACEMENT_3D('',#5645,#4605,#4606);
#3703=AXIS2_PLACEMENT_3D('',#5646,#4607,#4608);
#3704=AXIS2_PLACEMENT_3D('',#5647,#4609,#4610);
#3705=AXIS2_PLACEMENT_3D('',#5648,#4611,#4612);
#3706=AXIS2_PLACEMENT_3D('',#5649,#4613,#4614);
#3707=AXIS2_PLACEMENT_3D('',#5650,#4615,#4616);
#3708=AXIS2_PLACEMENT_3D('',#5651,#4617,#4618);
#3709=AXIS2_PLACEMENT_3D('',#5653,#4619,#4620);
#3710=AXIS2_PLACEMENT_3D('',#5656,#4622,#4623);
#3711=AXIS2_PLACEMENT_3D('',#5657,#4624,#4625);
#3712=AXIS2_PLACEMENT_3D('',#5659,#4626,#4627);
#3713=AXIS2_PLACEMENT_3D('',#5662,#4629,#4630);
#3714=AXIS2_PLACEMENT_3D('',#5663,#4631,#4632);
#3715=AXIS2_PLACEMENT_3D('',#5664,#4633,#4634);
#3716=AXIS2_PLACEMENT_3D('',#5665,#4635,#4636);
#3717=AXIS2_PLACEMENT_3D('',#5666,#4637,#4638);
#3718=AXIS2_PLACEMENT_3D('',#5668,#4639,#4640);
#3719=AXIS2_PLACEMENT_3D('',#5670,#4641,#4642);
#3720=AXIS2_PLACEMENT_3D('',#5671,#4643,#4644);
#3721=AXIS2_PLACEMENT_3D('',#5674,#4646,#4647);
#3722=AXIS2_PLACEMENT_3D('',#5675,#4648,#4649);
#3723=AXIS2_PLACEMENT_3D('',#5676,#4650,#4651);
#3724=AXIS2_PLACEMENT_3D('',#5678,#4652,#4653);
#3725=AXIS2_PLACEMENT_3D('',#5681,#4655,#4656);
#3726=AXIS2_PLACEMENT_3D('',#5682,#4657,#4658);
#3727=AXIS2_PLACEMENT_3D('',#5684,#4660,#4661);
#3728=AXIS2_PLACEMENT_3D('',#5686,#4662,#4663);
#3729=AXIS2_PLACEMENT_3D('',#5712,#4665,#4666);
#3730=AXIS2_PLACEMENT_3D('',#5718,#4670,#4671);
#3731=AXIS2_PLACEMENT_3D('',#5722,#4674,#4675);
#3732=AXIS2_PLACEMENT_3D('',#5726,#4678,#4679);
#3733=AXIS2_PLACEMENT_3D('',#5730,#4682,#4683);
#3734=AXIS2_PLACEMENT_3D('',#5734,#4686,#4687);
#3735=AXIS2_PLACEMENT_3D('',#5736,#4689,#4690);
#3736=AXIS2_PLACEMENT_3D('',#5737,#4691,#4692);
#3737=AXIS2_PLACEMENT_3D('',#5738,#4693,#4694);
#3738=AXIS2_PLACEMENT_3D('',#5739,#4695,#4696);
#3739=AXIS2_PLACEMENT_3D('',#5741,#4697,#4698);
#3740=AXIS2_PLACEMENT_3D('',#5744,#4700,#4701);
#3741=AXIS2_PLACEMENT_3D('',#5745,#4702,#4703);
#3742=AXIS2_PLACEMENT_3D('',#5747,#4704,#4705);
#3743=AXIS2_PLACEMENT_3D('',#5750,#4707,#4708);
#3744=AXIS2_PLACEMENT_3D('',#5751,#4709,#4710);
#3745=AXIS2_PLACEMENT_3D('',#5752,#4711,#4712);
#3746=AXIS2_PLACEMENT_3D('',#5753,#4713,#4714);
#3747=AXIS2_PLACEMENT_3D('',#5754,#4715,#4716);
#3748=AXIS2_PLACEMENT_3D('',#5766,#4718,#4719);
#3749=AXIS2_PLACEMENT_3D('',#5782,#4720,#4721);
#3750=AXIS2_PLACEMENT_3D('',#5784,#4722,#4723);
#3751=AXIS2_PLACEMENT_3D('',#5810,#4725,#4726);
#3752=AXIS2_PLACEMENT_3D('',#5813,#4729,#4730);
#3753=AXIS2_PLACEMENT_3D('',#5815,#4732,#4733);
#3754=AXIS2_PLACEMENT_3D('',#5817,#4735,#4736);
#3755=AXIS2_PLACEMENT_3D('',#5819,#4737,#4738);
#3756=AXIS2_PLACEMENT_3D('',#5822,#4740,#4741);
#3757=AXIS2_PLACEMENT_3D('',#5823,#4742,#4743);
#3758=AXIS2_PLACEMENT_3D('',#5825,#4745,#4746);
#3759=AXIS2_PLACEMENT_3D('',#5827,#4748,#4749);
#3760=AXIS2_PLACEMENT_3D('',#5828,#4750,#4751);
#3761=AXIS2_PLACEMENT_3D('',#5829,#4752,#4753);
#3762=AXIS2_PLACEMENT_3D('',#5830,#4754,#4755);
#3763=AXIS2_PLACEMENT_3D('',#5831,#4756,#4757);
#3764=AXIS2_PLACEMENT_3D('',#5832,#4758,#4759);
#3765=AXIS2_PLACEMENT_3D('',#5833,#4760,#4761);
#3766=AXIS2_PLACEMENT_3D('',#5834,#4762,#4763);
#3767=AXIS2_PLACEMENT_3D('',#5835,#4764,#4765);
#3768=AXIS2_PLACEMENT_3D('',#5836,#4766,#4767);
#3769=AXIS2_PLACEMENT_3D('',#5837,#4768,#4769);
#3770=AXIS2_PLACEMENT_3D('',#5838,#4770,#4771);
#3771=AXIS2_PLACEMENT_3D('',#5839,#4772,#4773);
#3772=AXIS2_PLACEMENT_3D('',#5840,#4774,#4775);
#3773=AXIS2_PLACEMENT_3D('',#5841,#4776,#4777);
#3774=AXIS2_PLACEMENT_3D('',#5842,#4778,#4779);
#3775=AXIS2_PLACEMENT_3D('',#5843,#4780,#4781);
#3776=AXIS2_PLACEMENT_3D('',#5844,#4782,#4783);
#3777=AXIS2_PLACEMENT_3D('',#5845,#4784,#4785);
#3778=AXIS2_PLACEMENT_3D('',#5846,#4786,#4787);
#3779=AXIS2_PLACEMENT_3D('',#5847,#4788,#4789);
#3780=AXIS2_PLACEMENT_3D('',#5848,#4790,#4791);
#3781=AXIS2_PLACEMENT_3D('',#5849,#4792,#4793);
#3782=AXIS2_PLACEMENT_3D('',#5850,#4794,#4795);
#3783=AXIS2_PLACEMENT_3D('',#5851,#4796,#4797);
#3784=AXIS2_PLACEMENT_3D('',#5852,#4798,#4799);
#3785=AXIS2_PLACEMENT_3D('',#5853,#4800,#4801);
#3786=AXIS2_PLACEMENT_3D('',#5854,#4802,#4803);
#3787=AXIS2_PLACEMENT_3D('',#5855,#4804,#4805);
#3788=AXIS2_PLACEMENT_3D('',#5856,#4806,#4807);
#3789=AXIS2_PLACEMENT_3D('',#5857,#4808,#4809);
#3790=AXIS2_PLACEMENT_3D('',#5858,#4810,#4811);
#3791=AXIS2_PLACEMENT_3D('',#5859,#4812,#4813);
#3792=AXIS2_PLACEMENT_3D('',#5860,#4814,#4815);
#3793=AXIS2_PLACEMENT_3D('',#5861,#4816,#4817);
#3794=AXIS2_PLACEMENT_3D('',#5862,#4818,#4819);
#3795=AXIS2_PLACEMENT_3D('',#5863,#4820,#4821);
#3796=AXIS2_PLACEMENT_3D('',#5864,#4822,#4823);
#3797=AXIS2_PLACEMENT_3D('',#5865,#4824,#4825);
#3798=AXIS2_PLACEMENT_3D('',#5866,#4826,#4827);
#3799=AXIS2_PLACEMENT_3D('',#5867,#4828,#4829);
#3800=AXIS2_PLACEMENT_3D('',#5868,#4830,#4831);
#3801=AXIS2_PLACEMENT_3D('',#5869,#4832,#4833);
#3802=AXIS2_PLACEMENT_3D('',#5870,#4834,#4835);
#3803=AXIS2_PLACEMENT_3D('',#5871,#4836,#4837);
#3804=AXIS2_PLACEMENT_3D('',#5872,#4838,#4839);
#3805=AXIS2_PLACEMENT_3D('',#5873,#4840,#4841);
#3806=AXIS2_PLACEMENT_3D('',#5874,#4842,#4843);
#3807=AXIS2_PLACEMENT_3D('',#5875,#4844,#4845);
#3808=AXIS2_PLACEMENT_3D('',#5876,#4846,#4847);
#3809=AXIS2_PLACEMENT_3D('',#5877,#4848,#4849);
#3810=AXIS2_PLACEMENT_3D('',#5878,#4850,#4851);
#3811=AXIS2_PLACEMENT_3D('',#5879,#4852,#4853);
#3812=AXIS2_PLACEMENT_3D('',#5880,#4854,#4855);
#3813=AXIS2_PLACEMENT_3D('',#5881,#4856,#4857);
#3814=DIRECTION('axis',(0.,0.,1.));
#3815=DIRECTION('refdir',(1.,0.,0.));
#3816=DIRECTION('axis',(0.,0.,1.));
#3817=DIRECTION('refdir',(1.,0.,0.));
#3818=DIRECTION('axis',(0.,0.,1.));
#3819=DIRECTION('refdir',(1.,0.,0.));
#3820=DIRECTION('center_axis',(0.,0.,1.));
#3821=DIRECTION('ref_axis',(1.,0.,0.));
#3822=DIRECTION('center_axis',(0.,0.,1.));
#3823=DIRECTION('ref_axis',(1.,0.,0.));
#3824=DIRECTION('',(0.,0.,1.));
#3825=DIRECTION('center_axis',(0.,0.,-1.));
#3826=DIRECTION('ref_axis',(1.,0.,0.));
#3827=DIRECTION('center_axis',(0.,0.,1.));
#3828=DIRECTION('ref_axis',(1.,0.,0.));
#3829=DIRECTION('center_axis',(0.,0.,1.));
#3830=DIRECTION('ref_axis',(1.,0.,0.));
#3831=DIRECTION('',(0.,0.,1.));
#3832=DIRECTION('center_axis',(0.,0.,-1.));
#3833=DIRECTION('ref_axis',(1.,0.,0.));
#3834=DIRECTION('center_axis',(0.,1.,0.));
#3835=DIRECTION('ref_axis',(1.,0.,0.));
#3836=DIRECTION('center_axis',(0.,1.,0.));
#3837=DIRECTION('ref_axis',(1.,0.,0.));
#3838=DIRECTION('',(0.,1.,0.));
#3839=DIRECTION('center_axis',(0.,-1.,0.));
#3840=DIRECTION('ref_axis',(1.,0.,0.));
#3841=DIRECTION('center_axis',(0.,1.,0.));
#3842=DIRECTION('ref_axis',(1.,0.,0.));
#3843=DIRECTION('center_axis',(0.,1.,0.));
#3844=DIRECTION('ref_axis',(1.,0.,0.));
#3845=DIRECTION('',(0.,1.,0.));
#3846=DIRECTION('center_axis',(0.,-1.,0.));
#3847=DIRECTION('ref_axis',(1.,0.,0.));
#3848=DIRECTION('center_axis',(0.,1.,0.));
#3849=DIRECTION('ref_axis',(-1.83697019872103E-16,0.,1.));
#3850=DIRECTION('',(0.,1.,0.));
#3851=DIRECTION('center_axis',(0.,1.,0.));
#3852=DIRECTION('ref_axis',(1.,0.,0.));
#3853=DIRECTION('',(0.,-1.,0.));
#3854=DIRECTION('center_axis',(0.,1.,0.));
#3855=DIRECTION('ref_axis',(1.,0.,0.));
#3856=DIRECTION('center_axis',(0.,1.,0.));
#3857=DIRECTION('ref_axis',(0.,0.,1.));
#3858=DIRECTION('',(0.,0.,-1.));
#3859=DIRECTION('',(-1.,0.,0.));
#3860=DIRECTION('',(0.,0.,-1.));
#3861=DIRECTION('',(1.,0.,0.));
#3862=DIRECTION('',(0.,0.,1.));
#3863=DIRECTION('center_axis',(1.,0.,0.));
#3864=DIRECTION('ref_axis',(0.,0.,-1.));
#3865=DIRECTION('',(0.,0.,1.));
#3866=DIRECTION('',(0.,1.,0.));
#3867=DIRECTION('center_axis',(0.,1.,0.));
#3868=DIRECTION('ref_axis',(1.,0.,0.));
#3869=DIRECTION('',(0.,0.,-1.));
#3870=DIRECTION('',(-1.,0.,0.));
#3871=DIRECTION('',(0.,0.,1.));
#3872=DIRECTION('',(1.,0.,0.));
#3873=DIRECTION('center_axis',(0.,0.,-1.));
#3874=DIRECTION('ref_axis',(-1.,0.,0.));
#3875=DIRECTION('',(0.,-1.,0.));
#3876=DIRECTION('center_axis',(-1.,0.,0.));
#3877=DIRECTION('ref_axis',(0.,0.,1.));
#3878=DIRECTION('',(0.,1.,0.));
#3879=DIRECTION('center_axis',(0.,0.,1.));
#3880=DIRECTION('ref_axis',(1.,0.,0.));
#3881=DIRECTION('',(0.,1.,0.));
#3882=DIRECTION('',(-1.,0.,0.));
#3883=DIRECTION('',(0.,-1.,0.));
#3884=DIRECTION('',(1.,0.,0.));
#3885=DIRECTION('',(0.,1.,0.));
#3886=DIRECTION('',(-1.,0.,0.));
#3887=DIRECTION('',(0.,1.,0.));
#3888=DIRECTION('',(1.,0.,0.));
#3889=DIRECTION('',(0.,1.,0.));
#3890=DIRECTION('center_axis',(0.,1.,0.));
#3891=DIRECTION('ref_axis',(-1.83697019872103E-16,0.,1.));
#3892=DIRECTION('',(0.,1.,0.));
#3893=DIRECTION('center_axis',(0.,1.,0.));
#3894=DIRECTION('ref_axis',(1.,0.,0.));
#3895=DIRECTION('',(0.,-1.,0.));
#3896=DIRECTION('center_axis',(0.,1.,0.));
#3897=DIRECTION('ref_axis',(1.,0.,0.));
#3898=DIRECTION('center_axis',(0.,1.,0.));
#3899=DIRECTION('ref_axis',(0.,0.,1.));
#3900=DIRECTION('',(0.,0.,-1.));
#3901=DIRECTION('',(-1.,0.,0.));
#3902=DIRECTION('',(0.,0.,-1.));
#3903=DIRECTION('',(0.,0.,1.));
#3904=DIRECTION('center_axis',(1.,0.,0.));
#3905=DIRECTION('ref_axis',(0.,0.,-1.));
#3906=DIRECTION('',(0.,0.,1.));
#3907=DIRECTION('',(0.,1.,0.));
#3908=DIRECTION('center_axis',(0.,1.,0.));
#3909=DIRECTION('ref_axis',(1.,0.,0.));
#3910=DIRECTION('',(0.,0.,-1.));
#3911=DIRECTION('',(0.,0.,1.));
#3912=DIRECTION('',(1.,0.,0.));
#3913=DIRECTION('center_axis',(0.,0.,-1.));
#3914=DIRECTION('ref_axis',(-1.,0.,0.));
#3915=DIRECTION('',(0.,-1.,0.));
#3916=DIRECTION('center_axis',(-1.,0.,0.));
#3917=DIRECTION('ref_axis',(0.,0.,1.));
#3918=DIRECTION('center_axis',(0.,1.,0.));
#3919=DIRECTION('ref_axis',(-1.,0.,0.));
#3920=DIRECTION('',(-1.,0.,0.));
#3921=DIRECTION('',(0.,0.,1.));
#3922=DIRECTION('',(0.,0.,1.));
#3923=DIRECTION('center_axis',(1.,0.,0.));
#3924=DIRECTION('ref_axis',(0.,1.,0.));
#3925=DIRECTION('',(0.,0.,1.));
#3926=DIRECTION('',(0.,1.,0.));
#3927=DIRECTION('center_axis',(0.,-1.,0.));
#3928=DIRECTION('ref_axis',(1.,0.,0.));
#3929=DIRECTION('',(1.,0.,0.));
#3930=DIRECTION('',(0.,0.,1.));
#3931=DIRECTION('center_axis',(-1.,0.,0.));
#3932=DIRECTION('ref_axis',(0.,-1.,0.));
#3933=DIRECTION('',(0.,-1.,0.));
#3934=DIRECTION('center_axis',(0.,0.,1.));
#3935=DIRECTION('ref_axis',(1.,0.,0.));
#3936=DIRECTION('axis',(0.,0.,1.));
#3937=DIRECTION('refdir',(1.,0.,0.));
#3938=DIRECTION('axis',(0.,0.,1.));
#3939=DIRECTION('refdir',(1.,0.,0.));
#3940=DIRECTION('center_axis',(-6.12323399573548E-17,1.,4.78224871431377E-30));
#3941=DIRECTION('ref_axis',(0.939692587475203,5.75395759716863E-17,0.342020234846066));
#3942=DIRECTION('center_axis',(-6.12323399573548E-17,1.,4.78224871431377E-30));
#3943=DIRECTION('ref_axis',(0.939692587475203,5.75395759716863E-17,0.342020234846066));
#3944=DIRECTION('',(-6.12323399573548E-17,1.,4.78224871431377E-30));
#3945=DIRECTION('center_axis',(6.12323399573548E-17,-1.,-4.78224871431377E-30));
#3946=DIRECTION('ref_axis',(0.939692587475203,5.75395759716863E-17,0.342020234846066));
#3947=DIRECTION('center_axis',(0.148462502781433,-0.987440631916705,0.0540359482919519));
#3948=DIRECTION('ref_axis',(0.927890642383958,0.157990501106673,0.337724676824699));
#3949=DIRECTION('center_axis',(6.12323399573548E-17,-1.,-4.78224871431377E-30));
#3950=DIRECTION('ref_axis',(0.939692587475203,5.75395759716863E-17,0.342020234846066));
#3951=DIRECTION('center_axis',(-6.12323399573548E-17,1.,4.78224871431377E-30));
#3952=DIRECTION('ref_axis',(0.939692587475203,5.75395759716863E-17,0.342020234846066));
#3953=DIRECTION('center_axis',(0.148462502781433,0.987440631916705,0.0540359482919519));
#3954=DIRECTION('ref_axis',(0.927890642383958,-0.157990501106673,0.337724676824699));
#3955=DIRECTION('center_axis',(-6.12323399573548E-17,1.,4.78224871431377E-30));
#3956=DIRECTION('ref_axis',(0.939692587475203,5.75395759716863E-17,0.342020234846066));
#3957=DIRECTION('',(-6.12323399573548E-17,1.,4.78224871431377E-30));
#3958=DIRECTION('center_axis',(6.12323399573548E-17,-1.,-4.78224871431377E-30));
#3959=DIRECTION('ref_axis',(0.939692587475203,5.75395759716863E-17,0.342020234846066));
#3960=DIRECTION('center_axis',(-6.12323399573548E-17,1.,4.78224871431377E-30));
#3961=DIRECTION('ref_axis',(0.939692587475203,5.75395759716863E-17,0.342020234846066));
#3962=DIRECTION('center_axis',(-6.12323399573548E-17,1.,4.78224871431377E-30));
#3963=DIRECTION('ref_axis',(0.939692587475203,5.75395759716863E-17,0.342020234846066));
#3964=DIRECTION('center_axis',(-6.12323399573548E-17,1.,4.78224871431377E-30));
#3965=DIRECTION('ref_axis',(0.939692587475203,5.75395759716863E-17,0.342020234846066));
#3966=DIRECTION('center_axis',(-0.148462502781433,0.987440631916705,-0.0540359482919519));
#3967=DIRECTION('ref_axis',(0.927890642383958,0.157990501106673,0.337724676824699));
#3968=DIRECTION('',(-6.12323399573548E-17,1.,4.78224871431377E-30));
#3969=DIRECTION('center_axis',(6.12323399573548E-17,-1.,-4.78224871431377E-30));
#3970=DIRECTION('ref_axis',(0.939692587475203,5.75395759716863E-17,0.342020234846066));
#3971=DIRECTION('center_axis',(-0.148462502781433,0.987440631916705,-0.0540359482919519));
#3972=DIRECTION('ref_axis',(0.927890642383958,0.157990501106673,0.337724676824699));
#3973=DIRECTION('center_axis',(-6.12323399573548E-17,1.,4.78224871431377E-30));
#3974=DIRECTION('ref_axis',(0.939692587475203,5.75395759716863E-17,0.342020234846066));
#3975=DIRECTION('center_axis',(-6.12323399573548E-17,1.,4.78224871431377E-30));
#3976=DIRECTION('ref_axis',(0.939692587475203,5.75395759716863E-17,0.342020234846066));
#3977=DIRECTION('',(-6.12323399573548E-17,1.,4.78224871431377E-30));
#3978=DIRECTION('center_axis',(-0.148462502781433,-0.987440631916705,-0.0540359482919519));
#3979=DIRECTION('ref_axis',(0.927890642383958,-0.157990501106673,0.337724676824699));
#3980=DIRECTION('center_axis',(6.12323399573548E-17,-1.,-4.78224871431377E-30));
#3981=DIRECTION('ref_axis',(0.939692587475203,5.75395759716863E-17,0.342020234846066));
#3982=DIRECTION('center_axis',(-0.148462502781433,-0.987440631916705,-0.0540359482919519));
#3983=DIRECTION('ref_axis',(0.927890642383958,-0.157990501106673,0.337724676824699));
#3984=DIRECTION('center_axis',(-6.12323399573548E-17,1.,4.78224871431377E-30));
#3985=DIRECTION('ref_axis',(0.939692587475203,5.75395759716863E-17,0.342020234846066));
#3986=DIRECTION('',(-0.342020234846066,-2.09426992923931E-17,0.939692587475203));
#3987=DIRECTION('center_axis',(-6.12323399573548E-17,1.,4.78224871431377E-30));
#3988=DIRECTION('ref_axis',(0.939692587475203,5.75395759716863E-17,0.342020234846066));
#3989=DIRECTION('',(-0.342020234846066,-2.09426992923931E-17,0.939692587475203));
#3990=DIRECTION('center_axis',(-6.12323399573548E-17,1.,4.78224871431377E-30));
#3991=DIRECTION('ref_axis',(0.939692587475203,5.75395759716863E-17,0.342020234846066));
#3992=DIRECTION('',(0.342020234846066,2.09426992923931E-17,-0.939692587475203));
#3993=DIRECTION('center_axis',(-6.12323399573548E-17,1.,4.78224871431377E-30));
#3994=DIRECTION('ref_axis',(0.939692587475203,5.75395759716863E-17,0.342020234846066));
#3995=DIRECTION('',(0.342020234846066,2.09426992923931E-17,-0.939692587475203));
#3996=DIRECTION('center_axis',(0.148462502781433,0.987440631916705,0.0540359482919519));
#3997=DIRECTION('ref_axis',(-0.927890642383958,0.157990501106673,-0.337724676824699));
#3998=DIRECTION('',(-0.342020234846066,-2.09426992923931E-17,0.939692587475203));
#3999=DIRECTION('',(-0.342020234846066,-2.09426992923931E-17,0.939692587475203));
#4000=DIRECTION('',(-0.927890642383958,0.157990501106673,-0.337724676824699));
#4001=DIRECTION('',(-0.342020234846066,-2.09426992923931E-17,0.939692587475203));
#4002=DIRECTION('center_axis',(0.148462502781433,0.987440631916705,0.0540359482919519));
#4003=DIRECTION('ref_axis',(0.927890642383958,-0.157990501106673,0.337724676824699));
#4004=DIRECTION('',(-0.927890642383958,0.157990501106673,-0.337724676824699));
#4005=DIRECTION('',(-0.342020234846066,-2.09426992923931E-17,0.939692587475203));
#4006=DIRECTION('center_axis',(0.148462502781433,-0.987440631916705,0.0540359482919519));
#4007=DIRECTION('ref_axis',(0.927890642383958,0.157990501106673,0.337724676824699));
#4008=DIRECTION('',(-0.342020234846066,-2.09426992923931E-17,0.939692587475203));
#4009=DIRECTION('',(0.927890642383958,0.157990501106673,0.337724676824699));
#4010=DIRECTION('center_axis',(0.148462502781433,-0.987440631916705,0.0540359482919519));
#4011=DIRECTION('ref_axis',(0.927890642383958,0.157990501106673,0.337724676824699));
#4012=DIRECTION('',(-0.342020234846066,-2.09426992923931E-17,0.939692587475203));
#4013=DIRECTION('',(0.927890642383958,0.157990501106673,0.337724676824699));
#4014=DIRECTION('',(-0.342020234846066,-2.09426992923931E-17,0.939692587475203));
#4015=DIRECTION('',(-0.342020234846066,-2.09426992923931E-17,0.939692587475203));
#4016=DIRECTION('center_axis',(-0.939692587475203,-5.75395759716863E-17,
-0.342020234846066));
#4017=DIRECTION('ref_axis',(6.12323399573548E-17,-1.,-4.78224871431377E-30));
#4018=DIRECTION('',(0.342020234846066,2.09426992923931E-17,-0.939692587475203));
#4019=DIRECTION('',(6.12323399573548E-17,-1.,-4.78224871431377E-30));
#4020=DIRECTION('',(-0.342020234846066,-2.09426992923931E-17,0.939692587475203));
#4021=DIRECTION('',(6.12323399573548E-17,-1.,-4.78224871431377E-30));
#4022=DIRECTION('center_axis',(0.939692587475203,5.75395759716863E-17,0.342020234846066));
#4023=DIRECTION('ref_axis',(-6.12323399573548E-17,1.,4.78224871431377E-30));
#4024=DIRECTION('',(-0.342020234846066,-2.09426992923931E-17,0.939692587475203));
#4025=DIRECTION('',(-6.12323399573548E-17,1.,4.78224871431377E-30));
#4026=DIRECTION('',(0.342020234846066,2.09426992923931E-17,-0.939692587475203));
#4027=DIRECTION('',(-6.12323399573548E-17,1.,4.78224871431377E-30));
#4028=DIRECTION('center_axis',(-0.342020234846066,-2.09426992923931E-17,
0.939692587475203));
#4029=DIRECTION('ref_axis',(0.939692587475203,5.75395759716863E-17,0.342020234846066));
#4030=DIRECTION('',(-0.927890642383958,-0.157990501106673,-0.337724676824699));
#4031=DIRECTION('',(0.927890642383958,-0.157990501106673,0.337724676824699));
#4032=DIRECTION('center_axis',(-6.12323399573548E-17,1.,4.78224871431377E-30));
#4033=DIRECTION('ref_axis',(0.939692587475203,5.75395759716863E-17,0.342020234846066));
#4034=DIRECTION('center_axis',(-6.12323399573548E-17,1.,4.78224871431377E-30));
#4035=DIRECTION('ref_axis',(0.939692587475203,5.75395759716863E-17,0.342020234846066));
#4036=DIRECTION('center_axis',(-6.12323399573548E-17,1.,4.78224871431377E-30));
#4037=DIRECTION('ref_axis',(0.939692587475203,5.75395759716863E-17,0.342020234846066));
#4038=DIRECTION('center_axis',(-6.12323399573548E-17,1.,4.78224871431377E-30));
#4039=DIRECTION('ref_axis',(0.939692587475203,5.75395759716863E-17,0.342020234846066));
#4040=DIRECTION('',(6.12323399573548E-17,-1.,-4.78224871431377E-30));
#4041=DIRECTION('center_axis',(-6.12323399573548E-17,1.,4.78224871431377E-30));
#4042=DIRECTION('ref_axis',(0.939692587475203,5.75395759716863E-17,0.342020234846066));
#4043=DIRECTION('',(-6.12323399573548E-17,1.,4.78224871431377E-30));
#4044=DIRECTION('center_axis',(-6.12323399573548E-17,1.,4.78224871431377E-30));
#4045=DIRECTION('ref_axis',(0.939692587475203,5.75395759716863E-17,0.342020234846066));
#4046=DIRECTION('center_axis',(-6.12323399573548E-17,1.,4.78224871431377E-30));
#4047=DIRECTION('ref_axis',(-0.939692587475203,-5.75395759716863E-17,-0.342020234846066));
#4048=DIRECTION('center_axis',(0.148462502781433,0.987440631916705,0.0540359482919519));
#4049=DIRECTION('ref_axis',(0.927890642383958,-0.157990501106673,0.337724676824699));
#4050=DIRECTION('center_axis',(-0.148462502781433,-0.987440631916705,-0.0540359482919519));
#4051=DIRECTION('ref_axis',(0.927890642383958,-0.157990501106673,0.337724676824699));
#4052=DIRECTION('',(-0.342020234846066,-2.09426992923931E-17,0.939692587475203));
#4053=DIRECTION('',(0.927890642383958,-0.157990501106673,0.337724676824699));
#4054=DIRECTION('',(0.927890642383958,-0.157990501106673,0.337724676824699));
#4055=DIRECTION('',(-0.342020234846066,-2.09426992923931E-17,0.939692587475203));
#4056=DIRECTION('',(0.927890642383958,-0.157990501106673,0.337724676824699));
#4057=DIRECTION('center_axis',(0.939692587475203,5.75395759716863E-17,0.342020234846066));
#4058=DIRECTION('ref_axis',(-6.12323399573548E-17,1.,4.78224871431377E-30));
#4059=DIRECTION('',(-6.12323399573548E-17,1.,4.78224871431377E-30));
#4060=DIRECTION('center_axis',(-0.939692587475203,-5.75395759716863E-17,
-0.342020234846066));
#4061=DIRECTION('ref_axis',(6.12323399573548E-17,-1.,-4.78224871431377E-30));
#4062=DIRECTION('',(6.12323399573548E-17,-1.,-4.78224871431377E-30));
#4063=DIRECTION('',(6.12323399573548E-17,-1.,-4.78224871431377E-30));
#4064=DIRECTION('center_axis',(-0.342020234846066,-2.09426992923931E-17,
0.939692587475203));
#4065=DIRECTION('ref_axis',(0.939692587475203,5.75395759716863E-17,0.342020234846066));
#4066=DIRECTION('',(-6.12323399573548E-17,1.,4.78224871431377E-30));
#4067=DIRECTION('center_axis',(-6.12323399573548E-17,1.,4.78224871431377E-30));
#4068=DIRECTION('ref_axis',(0.939692587475203,5.75395759716863E-17,0.342020234846066));
#4069=DIRECTION('center_axis',(-6.12323399573548E-17,1.,4.78224871431377E-30));
#4070=DIRECTION('ref_axis',(0.939692587475203,5.75395759716863E-17,0.342020234846066));
#4071=DIRECTION('center_axis',(-6.12323399573548E-17,1.,4.78224871431377E-30));
#4072=DIRECTION('ref_axis',(-0.939692587475203,-5.75395759716863E-17,-0.342020234846066));
#4073=DIRECTION('center_axis',(-6.12323399573548E-17,1.,4.78224871431377E-30));
#4074=DIRECTION('ref_axis',(0.939692587475203,5.75395759716863E-17,0.342020234846066));
#4075=DIRECTION('center_axis',(-6.12323399573548E-17,1.,4.78224871431377E-30));
#4076=DIRECTION('ref_axis',(0.939692587475203,5.75395759716863E-17,0.342020234846066));
#4077=DIRECTION('center_axis',(-0.148462502781433,0.987440631916705,-0.0540359482919519));
#4078=DIRECTION('ref_axis',(-0.927890642383958,-0.157990501106673,-0.337724676824699));
#4079=DIRECTION('',(-0.927890642383958,-0.157990501106673,-0.337724676824699));
#4080=DIRECTION('center_axis',(0.148462502781433,-0.987440631916705,0.0540359482919519));
#4081=DIRECTION('ref_axis',(0.927890642383958,0.157990501106673,0.337724676824699));
#4082=DIRECTION('',(-0.342020234846066,-2.09426992923931E-17,0.939692587475203));
#4083=DIRECTION('',(-0.927890642383958,-0.157990501106673,-0.337724676824699));
#4084=DIRECTION('',(-0.927890642383958,-0.157990501106673,-0.337724676824699));
#4085=DIRECTION('',(-0.342020234846066,-2.09426992923931E-17,0.939692587475203));
#4086=DIRECTION('center_axis',(-6.12323399573548E-17,1.,4.78224871431377E-30));
#4087=DIRECTION('ref_axis',(0.939692587475203,5.75395759716863E-17,0.342020234846066));
#4088=DIRECTION('center_axis',(-6.12323399573548E-17,1.,4.78224871431377E-30));
#4089=DIRECTION('ref_axis',(0.939692587475203,5.75395759716863E-17,0.342020234846066));
#4090=DIRECTION('center_axis',(-6.12323399573548E-17,1.,4.78224871431377E-30));
#4091=DIRECTION('ref_axis',(0.939692587475203,5.75395759716863E-17,0.342020234846066));
#4092=DIRECTION('center_axis',(-6.12323399573548E-17,1.,4.78224871431377E-30));
#4093=DIRECTION('ref_axis',(-0.939692587475202,-5.75395759716863E-17,-0.342020234846067));
#4094=DIRECTION('center_axis',(-6.12323399573548E-17,1.,4.78224871431377E-30));
#4095=DIRECTION('ref_axis',(0.939692587475203,5.75395759716863E-17,0.342020234846066));
#4096=DIRECTION('',(6.12323399573548E-17,-1.,-4.78224871431377E-30));
#4097=DIRECTION('',(-6.12323399573548E-17,1.,4.78224871431377E-30));
#4098=DIRECTION('center_axis',(-6.12323399573548E-17,1.,4.78224871431377E-30));
#4099=DIRECTION('ref_axis',(0.939692587475203,5.75395759716863E-17,0.342020234846066));
#4100=DIRECTION('center_axis',(-6.12323399573548E-17,1.,4.78224871431377E-30));
#4101=DIRECTION('ref_axis',(0.939692587475203,5.75395759716863E-17,0.342020234846066));
#4102=DIRECTION('center_axis',(0.939692587475203,5.75395759716863E-17,0.342020234846066));
#4103=DIRECTION('ref_axis',(-6.12323399573548E-17,1.,4.78224871431377E-30));
#4104=DIRECTION('',(-6.12323399573548E-17,1.,4.78224871431377E-30));
#4105=DIRECTION('center_axis',(-0.939692587475203,-5.75395759716863E-17,
-0.342020234846066));
#4106=DIRECTION('ref_axis',(6.12323399573548E-17,-1.,-4.78224871431377E-30));
#4107=DIRECTION('',(6.12323399573548E-17,-1.,-4.78224871431377E-30));
#4108=DIRECTION('',(6.12323399573548E-17,-1.,-4.78224871431377E-30));
#4109=DIRECTION('center_axis',(-0.342020234846066,-2.09426992923931E-17,
0.939692587475203));
#4110=DIRECTION('ref_axis',(0.939692587475203,5.75395759716863E-17,0.342020234846066));
#4111=DIRECTION('',(-6.12323399573548E-17,1.,4.78224871431377E-30));
#4112=DIRECTION('center_axis',(-0.342020234846066,-2.09426992923931E-17,
0.939692587475203));
#4113=DIRECTION('ref_axis',(0.939692587475203,5.75395759716863E-17,0.342020234846066));
#4114=DIRECTION('center_axis',(-6.12323399573548E-17,1.,4.78224871431377E-30));
#4115=DIRECTION('ref_axis',(0.939692587475203,5.75395759716863E-17,0.342020234846066));
#4116=DIRECTION('center_axis',(-6.12323399573548E-17,1.,4.78224871431377E-30));
#4117=DIRECTION('ref_axis',(0.939692587475203,5.75395759716863E-17,0.342020234846066));
#4118=DIRECTION('center_axis',(-6.12323399573548E-17,1.,4.78224871431377E-30));
#4119=DIRECTION('ref_axis',(0.939692587475203,5.75395759716863E-17,0.342020234846066));
#4120=DIRECTION('center_axis',(-6.12323399573548E-17,1.,4.78224871431377E-30));
#4121=DIRECTION('ref_axis',(0.939692587475203,5.75395759716863E-17,0.342020234846066));
#4122=DIRECTION('center_axis',(-6.12323399573548E-17,1.,4.78224871431377E-30));
#4123=DIRECTION('ref_axis',(-0.939692587475203,-5.75395759716863E-17,-0.342020234846066));
#4124=DIRECTION('axis',(0.,0.,1.));
#4125=DIRECTION('refdir',(1.,0.,0.));
#4126=DIRECTION('center_axis',(-6.12323399573548E-17,1.,4.78224871431377E-30));
#4127=DIRECTION('ref_axis',(0.939692587475203,5.75395759716863E-17,0.342020234846066));
#4128=DIRECTION('center_axis',(6.12323399573548E-17,-1.,-4.78224871431377E-30));
#4129=DIRECTION('ref_axis',(0.939692587475203,5.75395759716863E-17,0.342020234846066));
#4130=DIRECTION('',(6.12323399573548E-17,-1.,-4.78224871431377E-30));
#4131=DIRECTION('center_axis',(6.12323399573548E-17,-1.,-4.78224871431377E-30));
#4132=DIRECTION('ref_axis',(0.939692587475203,5.75395759716863E-17,0.342020234846066));
#4133=DIRECTION('center_axis',(-6.12323399573548E-17,1.,4.78224871431377E-30));
#4134=DIRECTION('ref_axis',(0.939692587475203,5.75395759716863E-17,0.342020234846066));
#4135=DIRECTION('center_axis',(-6.12323399573548E-17,1.,4.78224871431377E-30));
#4136=DIRECTION('ref_axis',(0.939692587475203,5.75395759716863E-17,0.342020234846066));
#4137=DIRECTION('',(6.12323399573548E-17,-1.,-4.78224871431377E-30));
#4138=DIRECTION('center_axis',(-6.12323399573548E-17,1.,4.78224871431377E-30));
#4139=DIRECTION('ref_axis',(0.939692587475203,5.75395759716863E-17,0.342020234846066));
#4140=DIRECTION('center_axis',(-6.12323399573548E-17,1.,4.78224871431377E-30));
#4141=DIRECTION('ref_axis',(0.939692587475203,5.75395759716863E-17,0.342020234846066));
#4142=DIRECTION('center_axis',(-6.12323399573548E-17,1.,4.78224871431377E-30));
#4143=DIRECTION('ref_axis',(0.939692587475203,5.75395759716863E-17,0.342020234846066));
#4144=DIRECTION('axis',(0.,0.,1.));
#4145=DIRECTION('refdir',(1.,0.,0.));
#4146=DIRECTION('center_axis',(-6.12323399573548E-17,1.,4.78224871431377E-30));
#4147=DIRECTION('ref_axis',(0.939692587475203,5.75395759716863E-17,0.342020234846066));
#4148=DIRECTION('center_axis',(-6.12323399573548E-17,1.,4.78224871431377E-30));
#4149=DIRECTION('ref_axis',(0.939692587475203,5.75395759716863E-17,0.342020234846066));
#4150=DIRECTION('center_axis',(-6.12323399573548E-17,1.,4.78224871431377E-30));
#4151=DIRECTION('ref_axis',(0.939692587475203,5.75395759716863E-17,0.342020234846066));
#4152=DIRECTION('center_axis',(-6.12323399573548E-17,1.,4.78224871431377E-30));
#4153=DIRECTION('ref_axis',(0.939692587475203,5.75395759716863E-17,0.342020234846066));
#4154=DIRECTION('',(6.12323399573548E-17,-1.,-4.78224871431377E-30));
#4155=DIRECTION('center_axis',(-6.12323399573548E-17,1.,4.78224871431377E-30));
#4156=DIRECTION('ref_axis',(0.939692587475203,5.75395759716863E-17,0.342020234846066));
#4157=DIRECTION('center_axis',(-6.12323399573548E-17,1.,4.78224871431377E-30));
#4158=DIRECTION('ref_axis',(0.939692587475203,5.75395759716863E-17,0.342020234846066));
#4159=DIRECTION('center_axis',(6.12323399573548E-17,-1.,-4.78224871431377E-30));
#4160=DIRECTION('ref_axis',(0.939692587475203,5.75395759716863E-17,0.342020234846066));
#4161=DIRECTION('center_axis',(-6.12323399573548E-17,1.,4.78224871431377E-30));
#4162=DIRECTION('ref_axis',(0.939692587475203,5.75395759716863E-17,0.342020234846066));
#4163=DIRECTION('',(-6.12323399573548E-17,1.,4.78224871431377E-30));
#4164=DIRECTION('center_axis',(6.12323399573548E-17,-1.,-4.78224871431377E-30));
#4165=DIRECTION('ref_axis',(0.939692587475203,5.75395759716863E-17,0.342020234846066));
#4166=DIRECTION('center_axis',(-6.12323399573548E-17,1.,4.78224871431377E-30));
#4167=DIRECTION('ref_axis',(0.939692587475203,5.75395759716863E-17,0.342020234846066));
#4168=DIRECTION('',(-0.664463000834449,0.707106781186548,-0.241844827362669));
#4169=DIRECTION('center_axis',(6.12323399573548E-17,-1.,-4.78224871431377E-30));
#4170=DIRECTION('ref_axis',(0.939692587475203,5.75395759716863E-17,0.342020234846066));
#4171=DIRECTION('center_axis',(-6.12323399573548E-17,1.,4.78224871431377E-30));
#4172=DIRECTION('ref_axis',(0.939692587475203,5.75395759716863E-17,0.342020234846066));
#4173=DIRECTION('',(-0.813797652501456,-0.5,-0.296198211985013));
#4174=DIRECTION('center_axis',(0.342020234846066,2.09426992923931E-17,-0.939692587475203));
#4175=DIRECTION('ref_axis',(-0.939692587475203,-5.75395759716863E-17,-0.342020234846066));
#4176=DIRECTION('',(-6.12323399573548E-17,1.,4.78224871431377E-30));
#4177=DIRECTION('',(-0.939692587475203,-5.75395759716863E-17,-0.342020234846066));
#4178=DIRECTION('',(-6.12323399573548E-17,1.,4.78224871431377E-30));
#4179=DIRECTION('center_axis',(0.98480776992449,6.03020841606616E-17,-0.173648081752589));
#4180=DIRECTION('ref_axis',(-0.173648081752589,-1.06328783748123E-17,-0.98480776992449));
#4181=DIRECTION('',(-6.12323399573548E-17,1.,4.78224871431377E-30));
#4182=DIRECTION('',(-0.173648081752589,-1.06328783748123E-17,-0.98480776992449));
#4183=DIRECTION('center_axis',(0.642787535078424,3.93593848682685E-17,0.766044505722614));
#4184=DIRECTION('ref_axis',(0.766044505722614,4.6906697596874E-17,-0.642787535078424));
#4185=DIRECTION('',(-6.12323399573548E-17,1.,4.78224871431377E-30));
#4186=DIRECTION('',(0.766044505722614,4.6906697596874E-17,-0.642787535078424));
#4187=DIRECTION('center_axis',(-0.342020234846066,-2.09426992923931E-17,
0.939692587475203));
#4188=DIRECTION('ref_axis',(0.939692587475203,5.75395759716863E-17,0.342020234846066));
#4189=DIRECTION('',(-6.12323399573548E-17,1.,4.78224871431377E-30));
#4190=DIRECTION('',(0.939692587475203,5.75395759716863E-17,0.342020234846066));
#4191=DIRECTION('center_axis',(-0.98480776992449,-6.03020841606616E-17,
0.173648081752588));
#4192=DIRECTION('ref_axis',(0.173648081752588,1.06328783748123E-17,0.98480776992449));
#4193=DIRECTION('',(-6.12323399573548E-17,1.,4.78224871431377E-30));
#4194=DIRECTION('',(0.173648081752588,1.06328783748123E-17,0.98480776992449));
#4195=DIRECTION('center_axis',(-0.642787535078423,-3.93593848682685E-17,
-0.766044505722615));
#4196=DIRECTION('ref_axis',(-0.766044505722615,-4.6906697596874E-17,0.642787535078423));
#4197=DIRECTION('',(-0.766044505722615,-4.6906697596874E-17,0.642787535078423));
#4198=DIRECTION('center_axis',(-6.12323399573548E-17,1.,4.78224871431377E-30));
#4199=DIRECTION('ref_axis',(-0.342020234846066,-2.09426992923931E-17,0.939692587475203));
#4200=DIRECTION('center_axis',(-6.12323399573548E-17,1.,4.78224871431377E-30));
#4201=DIRECTION('ref_axis',(0.939692587475203,5.75395759716863E-17,0.342020234846066));
#4202=DIRECTION('axis',(0.,0.,1.));
#4203=DIRECTION('refdir',(1.,0.,0.));
#4204=DIRECTION('center_axis',(-6.12323399573548E-17,1.,4.78224871431377E-30));
#4205=DIRECTION('ref_axis',(0.939692587475203,5.75395759716863E-17,0.342020234846066));
#4206=DIRECTION('center_axis',(6.12323399573548E-17,-1.,-4.78224871431377E-30));
#4207=DIRECTION('ref_axis',(0.939692587475203,5.75395759716863E-17,0.342020234846066));
#4208=DIRECTION('',(6.12323399573548E-17,-1.,-4.78224871431377E-30));
#4209=DIRECTION('center_axis',(6.12323399573548E-17,-1.,-4.78224871431377E-30));
#4210=DIRECTION('ref_axis',(0.939692587475203,5.75395759716863E-17,0.342020234846066));
#4211=DIRECTION('center_axis',(-6.12323399573548E-17,1.,4.78224871431377E-30));
#4212=DIRECTION('ref_axis',(0.939692587475203,5.75395759716863E-17,0.342020234846066));
#4213=DIRECTION('center_axis',(-6.12323399573548E-17,1.,4.78224871431377E-30));
#4214=DIRECTION('ref_axis',(0.939692587475203,5.75395759716863E-17,0.342020234846066));
#4215=DIRECTION('',(6.12323399573548E-17,-1.,-4.78224871431377E-30));
#4216=DIRECTION('center_axis',(-6.12323399573548E-17,1.,4.78224871431377E-30));
#4217=DIRECTION('ref_axis',(0.939692587475203,5.75395759716863E-17,0.342020234846066));
#4218=DIRECTION('center_axis',(-6.12323399573548E-17,1.,4.78224871431377E-30));
#4219=DIRECTION('ref_axis',(0.939692587475203,5.75395759716863E-17,0.342020234846066));
#4220=DIRECTION('center_axis',(-6.12323399573548E-17,1.,4.78224871431377E-30));
#4221=DIRECTION('ref_axis',(0.939692587475203,5.75395759716863E-17,0.342020234846066));
#4222=DIRECTION('axis',(0.,0.,1.));
#4223=DIRECTION('refdir',(1.,0.,0.));
#4224=DIRECTION('center_axis',(-6.12323399573548E-17,1.,4.78224871431377E-30));
#4225=DIRECTION('ref_axis',(0.939692587475203,5.75395759716863E-17,0.342020234846066));
#4226=DIRECTION('center_axis',(6.12323399573548E-17,-1.,-4.78224871431377E-30));
#4227=DIRECTION('ref_axis',(0.939692587475203,5.75395759716863E-17,0.342020234846066));
#4228=DIRECTION('',(6.12323399573548E-17,-1.,-4.78224871431377E-30));
#4229=DIRECTION('center_axis',(6.12323399573548E-17,-1.,-4.78224871431377E-30));
#4230=DIRECTION('ref_axis',(0.939692587475203,5.75395759716863E-17,0.342020234846066));
#4231=DIRECTION('center_axis',(-6.12323399573548E-17,1.,4.78224871431377E-30));
#4232=DIRECTION('ref_axis',(0.939692587475203,5.75395759716863E-17,0.342020234846066));
#4233=DIRECTION('center_axis',(-6.12323399573548E-17,1.,4.78224871431377E-30));
#4234=DIRECTION('ref_axis',(0.939692587475203,5.75395759716863E-17,0.342020234846066));
#4235=DIRECTION('',(6.12323399573548E-17,-1.,-4.78224871431377E-30));
#4236=DIRECTION('center_axis',(-6.12323399573548E-17,1.,4.78224871431377E-30));
#4237=DIRECTION('ref_axis',(0.939692587475203,5.75395759716863E-17,0.342020234846066));
#4238=DIRECTION('center_axis',(-6.12323399573548E-17,1.,4.78224871431377E-30));
#4239=DIRECTION('ref_axis',(0.939692587475203,5.75395759716863E-17,0.342020234846066));
#4240=DIRECTION('center_axis',(-6.12323399573548E-17,1.,4.78224871431377E-30));
#4241=DIRECTION('ref_axis',(0.939692587475203,5.75395759716863E-17,0.342020234846066));
#4242=DIRECTION('axis',(0.,0.,1.));
#4243=DIRECTION('refdir',(1.,0.,0.));
#4244=DIRECTION('center_axis',(-6.12323399573548E-17,1.,4.78224871431377E-30));
#4245=DIRECTION('ref_axis',(0.939692587475203,5.75395759716863E-17,0.342020234846066));
#4246=DIRECTION('',(0.813797652501457,-0.5,0.296198211985013));
#4247=DIRECTION('center_axis',(6.12323399573548E-17,-1.,-4.78224871431377E-30));
#4248=DIRECTION('ref_axis',(0.939692587475203,5.75395759716863E-17,0.342020234846066));
#4249=DIRECTION('center_axis',(6.12323399573548E-17,-1.,-4.78224871431377E-30));
#4250=DIRECTION('ref_axis',(0.939692587475203,5.75395759716863E-17,0.342020234846066));
#4251=DIRECTION('center_axis',(-6.12323399573548E-17,1.,4.78224871431377E-30));
#4252=DIRECTION('ref_axis',(0.939692587475203,5.75395759716863E-17,0.342020234846066));
#4253=DIRECTION('',(-0.813797652501456,-0.5,-0.296198211985013));
#4254=DIRECTION('center_axis',(0.342020234846066,2.09426992923931E-17,-0.939692587475203));
#4255=DIRECTION('ref_axis',(-0.939692587475203,-5.75395759716863E-17,-0.342020234846066));
#4256=DIRECTION('',(-6.12323399573548E-17,1.,4.78224871431377E-30));
#4257=DIRECTION('',(-6.12323399573548E-17,1.,4.78224871431377E-30));
#4258=DIRECTION('center_axis',(-0.642787535078423,-3.93593848682685E-17,
-0.766044505722615));
#4259=DIRECTION('ref_axis',(-0.766044505722615,-4.6906697596874E-17,0.642787535078423));
#4260=DIRECTION('',(-6.12323399573548E-17,1.,4.78224871431377E-30));
#4261=DIRECTION('center_axis',(-0.98480776992449,-6.03020841606616E-17,
0.173648081752588));
#4262=DIRECTION('ref_axis',(0.173648081752588,1.06328783748123E-17,0.98480776992449));
#4263=DIRECTION('',(-6.12323399573548E-17,1.,4.78224871431377E-30));
#4264=DIRECTION('center_axis',(-6.12323399573548E-17,1.,4.78224871431377E-30));
#4265=DIRECTION('ref_axis',(0.939692587475203,5.75395759716863E-17,0.342020234846066));
#4266=DIRECTION('center_axis',(-6.12323399573548E-17,1.,4.78224871431377E-30));
#4267=DIRECTION('ref_axis',(0.939692587475203,5.75395759716863E-17,0.342020234846066));
#4268=DIRECTION('',(6.12323399573548E-17,-1.,-4.78224871431377E-30));
#4269=DIRECTION('center_axis',(-6.12323399573548E-17,1.,4.78224871431377E-30));
#4270=DIRECTION('ref_axis',(0.939692587475203,5.75395759716863E-17,0.342020234846066));
#4271=DIRECTION('center_axis',(-0.342020234846066,-2.09426992923931E-17,
0.939692587475203));
#4272=DIRECTION('ref_axis',(0.939692587475203,5.75395759716863E-17,0.342020234846066));
#4273=DIRECTION('',(-6.12323399573548E-17,1.,4.78224871431377E-30));
#4274=DIRECTION('center_axis',(0.98480776992449,6.03020841606616E-17,-0.173648081752589));
#4275=DIRECTION('ref_axis',(-0.173648081752589,-1.06328783748123E-17,-0.98480776992449));
#4276=DIRECTION('',(-6.12323399573548E-17,1.,4.78224871431377E-30));
#4277=DIRECTION('center_axis',(0.642787535078424,3.93593848682685E-17,0.766044505722614));
#4278=DIRECTION('ref_axis',(0.766044505722614,4.6906697596874E-17,-0.642787535078424));
#4279=DIRECTION('center_axis',(-6.12323399573548E-17,1.,4.78224871431377E-30));
#4280=DIRECTION('ref_axis',(0.939692587475203,5.75395759716863E-17,0.342020234846066));
#4281=DIRECTION('center_axis',(-6.12323399573548E-17,1.,4.78224871431377E-30));
#4282=DIRECTION('ref_axis',(0.939692587475203,5.75395759716863E-17,0.342020234846066));
#4283=DIRECTION('',(0.,0.,1.));
#4284=DIRECTION('',(1.,0.,0.));
#4285=DIRECTION('',(0.,0.,1.));
#4286=DIRECTION('',(1.,0.,0.));
#4287=DIRECTION('',(0.,0.,1.));
#4288=DIRECTION('',(1.,0.,0.));
#4289=DIRECTION('',(0.,0.,1.));
#4290=DIRECTION('',(1.,0.,0.));
#4291=DIRECTION('',(0.,0.,1.));
#4292=DIRECTION('',(1.,0.,0.));
#4293=DIRECTION('',(0.,0.,1.));
#4294=DIRECTION('',(1.,0.,0.));
#4295=DIRECTION('axis',(0.,0.,1.));
#4296=DIRECTION('refdir',(1.,0.,0.));
#4297=DIRECTION('axis',(0.,0.,1.));
#4298=DIRECTION('refdir',(1.,0.,0.));
#4299=DIRECTION('axis',(0.,0.,1.));
#4300=DIRECTION('refdir',(1.,0.,0.));
#4301=DIRECTION('axis',(0.,0.,1.));
#4302=DIRECTION('refdir',(1.,0.,0.));
#4303=DIRECTION('axis',(0.,0.,1.));
#4304=DIRECTION('refdir',(1.,0.,0.));
#4305=DIRECTION('axis',(0.,0.,1.));
#4306=DIRECTION('refdir',(1.,0.,0.));
#4307=DIRECTION('axis',(0.,0.,1.));
#4308=DIRECTION('refdir',(1.,0.,0.));
#4309=DIRECTION('center_axis',(0.,0.,1.));
#4310=DIRECTION('ref_axis',(1.,0.,0.));
#4311=DIRECTION('center_axis',(0.,0.,1.));
#4312=DIRECTION('ref_axis',(1.,0.,0.));
#4313=DIRECTION('',(0.,0.,1.));
#4314=DIRECTION('center_axis',(0.,0.,-1.));
#4315=DIRECTION('ref_axis',(1.,0.,0.));
#4316=DIRECTION('center_axis',(0.,0.,1.));
#4317=DIRECTION('ref_axis',(1.,0.,0.));
#4318=DIRECTION('center_axis',(0.,0.,1.));
#4319=DIRECTION('ref_axis',(1.,0.,0.));
#4320=DIRECTION('',(0.,0.,1.));
#4321=DIRECTION('center_axis',(0.,0.,-1.));
#4322=DIRECTION('ref_axis',(1.,0.,0.));
#4323=DIRECTION('center_axis',(0.,1.,0.));
#4324=DIRECTION('ref_axis',(1.,0.,0.));
#4325=DIRECTION('center_axis',(0.,1.,0.));
#4326=DIRECTION('ref_axis',(1.,0.,0.));
#4327=DIRECTION('',(0.,1.,0.));
#4328=DIRECTION('center_axis',(0.,-1.,0.));
#4329=DIRECTION('ref_axis',(1.,0.,0.));
#4330=DIRECTION('center_axis',(0.,1.,0.));
#4331=DIRECTION('ref_axis',(1.,0.,0.));
#4332=DIRECTION('center_axis',(0.,1.,0.));
#4333=DIRECTION('ref_axis',(1.,0.,0.));
#4334=DIRECTION('',(0.,1.,0.));
#4335=DIRECTION('center_axis',(0.,-1.,0.));
#4336=DIRECTION('ref_axis',(1.,0.,0.));
#4337=DIRECTION('center_axis',(0.,1.,0.));
#4338=DIRECTION('ref_axis',(-1.83697019872103E-16,0.,1.));
#4339=DIRECTION('',(0.,1.,0.));
#4340=DIRECTION('center_axis',(0.,1.,0.));
#4341=DIRECTION('ref_axis',(1.,0.,0.));
#4342=DIRECTION('',(0.,-1.,0.));
#4343=DIRECTION('center_axis',(0.,1.,0.));
#4344=DIRECTION('ref_axis',(1.,0.,0.));
#4345=DIRECTION('center_axis',(0.,1.,0.));
#4346=DIRECTION('ref_axis',(0.,0.,1.));
#4347=DIRECTION('',(0.,0.,-1.));
#4348=DIRECTION('',(1.,0.,0.));
#4349=DIRECTION('',(0.,0.,1.));
#4350=DIRECTION('',(-1.,0.,0.));
#4351=DIRECTION('',(0.,0.,1.));
#4352=DIRECTION('center_axis',(1.,0.,0.));
#4353=DIRECTION('ref_axis',(0.,0.,-1.));
#4354=DIRECTION('',(0.,0.,1.));
#4355=DIRECTION('',(0.,-1.,0.));
#4356=DIRECTION('center_axis',(0.,1.,0.));
#4357=DIRECTION('ref_axis',(1.,0.,0.));
#4358=DIRECTION('',(0.,0.,-1.));
#4359=DIRECTION('',(1.,0.,0.));
#4360=DIRECTION('',(0.,0.,-1.));
#4361=DIRECTION('',(-1.,0.,0.));
#4362=DIRECTION('center_axis',(-1.,0.,0.));
#4363=DIRECTION('ref_axis',(0.,0.,1.));
#4364=DIRECTION('',(0.,1.,0.));
#4365=DIRECTION('center_axis',(0.,0.,-1.));
#4366=DIRECTION('ref_axis',(-1.,0.,0.));
#4367=DIRECTION('',(0.,1.,0.));
#4368=DIRECTION('center_axis',(-1.,0.,0.));
#4369=DIRECTION('ref_axis',(0.,-1.,0.));
#4370=DIRECTION('',(0.,-1.,0.));
#4371=DIRECTION('',(0.,0.,1.));
#4372=DIRECTION('',(0.,-1.,0.));
#4373=DIRECTION('',(0.,0.,1.));
#4374=DIRECTION('',(0.,-1.,0.));
#4375=DIRECTION('',(0.,0.,-1.));
#4376=DIRECTION('',(0.,1.,0.));
#4377=DIRECTION('',(0.,0.,1.));
#4378=DIRECTION('',(0.,-1.,0.));
#4379=DIRECTION('center_axis',(0.,1.,0.));
#4380=DIRECTION('ref_axis',(-1.83697019872103E-16,0.,1.));
#4381=DIRECTION('',(0.,1.,0.));
#4382=DIRECTION('center_axis',(0.,1.,0.));
#4383=DIRECTION('ref_axis',(1.,0.,0.));
#4384=DIRECTION('',(0.,-1.,0.));
#4385=DIRECTION('center_axis',(0.,1.,0.));
#4386=DIRECTION('ref_axis',(1.,0.,0.));
#4387=DIRECTION('center_axis',(0.,1.,0.));
#4388=DIRECTION('ref_axis',(0.,0.,1.));
#4389=DIRECTION('',(0.,0.,-1.));
#4390=DIRECTION('',(1.,0.,0.));
#4391=DIRECTION('',(-1.,0.,0.));
#4392=DIRECTION('',(0.,0.,1.));
#4393=DIRECTION('center_axis',(1.,0.,0.));
#4394=DIRECTION('ref_axis',(0.,0.,-1.));
#4395=DIRECTION('',(0.,0.,1.));
#4396=DIRECTION('',(0.,-1.,0.));
#4397=DIRECTION('center_axis',(0.,1.,0.));
#4398=DIRECTION('ref_axis',(1.,0.,0.));
#4399=DIRECTION('',(0.,0.,-1.));
#4400=DIRECTION('',(1.,0.,0.));
#4401=DIRECTION('',(-1.,0.,0.));
#4402=DIRECTION('center_axis',(-1.,0.,0.));
#4403=DIRECTION('ref_axis',(0.,0.,1.));
#4404=DIRECTION('',(0.,1.,0.));
#4405=DIRECTION('center_axis',(0.,0.,-1.));
#4406=DIRECTION('ref_axis',(-1.,0.,0.));
#4407=DIRECTION('center_axis',(0.,1.,0.));
#4408=DIRECTION('ref_axis',(-1.,0.,0.));
#4409=DIRECTION('',(-1.,0.,0.));
#4410=DIRECTION('',(-1.,0.,0.));
#4411=DIRECTION('',(0.,0.,1.));
#4412=DIRECTION('center_axis',(1.,0.,0.));
#4413=DIRECTION('ref_axis',(0.,1.,0.));
#4414=DIRECTION('',(0.,1.,0.));
#4415=DIRECTION('',(0.,1.,0.));
#4416=DIRECTION('',(0.,0.,1.));
#4417=DIRECTION('center_axis',(0.,-1.,0.));
#4418=DIRECTION('ref_axis',(1.,0.,0.));
#4419=DIRECTION('',(1.,0.,0.));
#4420=DIRECTION('',(1.,0.,0.));
#4421=DIRECTION('center_axis',(0.,0.,1.));
#4422=DIRECTION('ref_axis',(1.,0.,0.));
#4423=DIRECTION('center_axis',(0.,0.,1.));
#4424=DIRECTION('ref_axis',(1.,0.,0.));
#4425=DIRECTION('',(0.,0.,1.));
#4426=DIRECTION('',(1.,0.,0.));
#4427=DIRECTION('axis',(0.,0.,1.));
#4428=DIRECTION('refdir',(1.,0.,0.));
#4429=DIRECTION('axis',(0.,0.,1.));
#4430=DIRECTION('refdir',(1.,0.,0.));
#4431=DIRECTION('center_axis',(0.,1.,0.));
#4432=DIRECTION('ref_axis',(1.,0.,0.));
#4433=DIRECTION('center_axis',(0.,1.,0.));
#4434=DIRECTION('ref_axis',(1.,0.,0.));
#4435=DIRECTION('',(0.,1.,0.));
#4436=DIRECTION('center_axis',(0.,-1.,0.));
#4437=DIRECTION('ref_axis',(1.,0.,0.));
#4438=DIRECTION('center_axis',(0.157990501106673,-0.987440631916705,0.));
#4439=DIRECTION('ref_axis',(0.987440631916705,0.157990501106673,0.));
#4440=DIRECTION('center_axis',(0.,-1.,0.));
#4441=DIRECTION('ref_axis',(1.,0.,0.));
#4442=DIRECTION('center_axis',(0.,1.,0.));
#4443=DIRECTION('ref_axis',(1.,0.,0.));
#4444=DIRECTION('center_axis',(0.157990501106673,0.987440631916705,0.));
#4445=DIRECTION('ref_axis',(0.987440631916705,-0.157990501106673,0.));
#4446=DIRECTION('center_axis',(0.,1.,0.));
#4447=DIRECTION('ref_axis',(1.,0.,0.));
#4448=DIRECTION('',(0.,1.,0.));
#4449=DIRECTION('center_axis',(0.,-1.,0.));
#4450=DIRECTION('ref_axis',(1.,0.,0.));
#4451=DIRECTION('center_axis',(0.,1.,0.));
#4452=DIRECTION('ref_axis',(1.,0.,0.));
#4453=DIRECTION('center_axis',(0.,1.,0.));
#4454=DIRECTION('ref_axis',(1.,0.,0.));
#4455=DIRECTION('center_axis',(0.,1.,0.));
#4456=DIRECTION('ref_axis',(1.,0.,0.));
#4457=DIRECTION('center_axis',(-0.157990501106673,0.987440631916705,0.));
#4458=DIRECTION('ref_axis',(0.987440631916705,0.157990501106673,0.));
#4459=DIRECTION('',(0.,1.,0.));
#4460=DIRECTION('center_axis',(0.,-1.,0.));
#4461=DIRECTION('ref_axis',(1.,0.,0.));
#4462=DIRECTION('center_axis',(-0.157990501106673,0.987440631916705,0.));
#4463=DIRECTION('ref_axis',(0.987440631916705,0.157990501106673,0.));
#4464=DIRECTION('center_axis',(0.,1.,0.));
#4465=DIRECTION('ref_axis',(1.,0.,0.));
#4466=DIRECTION('center_axis',(0.,1.,0.));
#4467=DIRECTION('ref_axis',(1.,0.,0.));
#4468=DIRECTION('',(0.,1.,0.));
#4469=DIRECTION('center_axis',(-0.157990501106673,-0.987440631916705,0.));
#4470=DIRECTION('ref_axis',(0.987440631916705,-0.157990501106673,0.));
#4471=DIRECTION('center_axis',(0.,-1.,0.));
#4472=DIRECTION('ref_axis',(1.,0.,0.));
#4473=DIRECTION('center_axis',(-0.157990501106673,-0.987440631916705,0.));
#4474=DIRECTION('ref_axis',(0.987440631916705,-0.157990501106673,0.));
#4475=DIRECTION('center_axis',(0.,1.,0.));
#4476=DIRECTION('ref_axis',(1.,0.,0.));
#4477=DIRECTION('',(0.,0.,1.));
#4478=DIRECTION('center_axis',(0.,1.,0.));
#4479=DIRECTION('ref_axis',(1.,0.,0.));
#4480=DIRECTION('',(0.,0.,1.));
#4481=DIRECTION('center_axis',(0.,1.,0.));
#4482=DIRECTION('ref_axis',(1.,0.,0.));
#4483=DIRECTION('',(0.,0.,-1.));
#4484=DIRECTION('center_axis',(0.,1.,0.));
#4485=DIRECTION('ref_axis',(1.,0.,0.));
#4486=DIRECTION('',(0.,0.,-1.));
#4487=DIRECTION('center_axis',(0.157990501106673,0.987440631916705,0.));
#4488=DIRECTION('ref_axis',(-0.987440631916705,0.157990501106673,0.));
#4489=DIRECTION('',(0.,0.,1.));
#4490=DIRECTION('',(0.,0.,1.));
#4491=DIRECTION('',(-0.987440631916705,0.157990501106673,0.));
#4492=DIRECTION('',(0.,0.,1.));
#4493=DIRECTION('center_axis',(0.157990501106673,0.987440631916705,0.));
#4494=DIRECTION('ref_axis',(0.987440631916705,-0.157990501106673,0.));
#4495=DIRECTION('',(-0.987440631916705,0.157990501106673,0.));
#4496=DIRECTION('',(0.,0.,1.));
#4497=DIRECTION('center_axis',(0.157990501106673,-0.987440631916705,0.));
#4498=DIRECTION('ref_axis',(0.987440631916705,0.157990501106673,0.));
#4499=DIRECTION('',(0.,0.,1.));
#4500=DIRECTION('',(0.987440631916705,0.157990501106673,0.));
#4501=DIRECTION('center_axis',(0.157990501106673,-0.987440631916705,0.));
#4502=DIRECTION('ref_axis',(0.987440631916705,0.157990501106673,0.));
#4503=DIRECTION('',(0.,0.,1.));
#4504=DIRECTION('',(0.987440631916705,0.157990501106673,0.));
#4505=DIRECTION('',(0.,0.,1.));
#4506=DIRECTION('',(0.,0.,1.));
#4507=DIRECTION('center_axis',(-1.,0.,0.));
#4508=DIRECTION('ref_axis',(0.,-1.,0.));
#4509=DIRECTION('',(0.,0.,-1.));
#4510=DIRECTION('',(0.,-1.,0.));
#4511=DIRECTION('',(0.,0.,1.));
#4512=DIRECTION('',(0.,-1.,0.));
#4513=DIRECTION('center_axis',(1.,0.,0.));
#4514=DIRECTION('ref_axis',(0.,1.,0.));
#4515=DIRECTION('',(0.,0.,1.));
#4516=DIRECTION('',(0.,1.,0.));
#4517=DIRECTION('',(0.,0.,-1.));
#4518=DIRECTION('',(0.,1.,0.));
#4519=DIRECTION('center_axis',(0.,0.,1.));
#4520=DIRECTION('ref_axis',(1.,0.,0.));
#4521=DIRECTION('',(-0.987440631916705,-0.157990501106673,0.));
#4522=DIRECTION('',(0.987440631916705,-0.157990501106673,0.));
#4523=DIRECTION('center_axis',(0.,1.,0.));
#4524=DIRECTION('ref_axis',(1.,0.,0.));
#4525=DIRECTION('center_axis',(0.,1.,0.));
#4526=DIRECTION('ref_axis',(1.,0.,0.));
#4527=DIRECTION('center_axis',(0.,1.,0.));
#4528=DIRECTION('ref_axis',(1.,0.,0.));
#4529=DIRECTION('center_axis',(0.,1.,0.));
#4530=DIRECTION('ref_axis',(1.,0.,0.));
#4531=DIRECTION('',(0.,-1.,0.));
#4532=DIRECTION('center_axis',(0.,1.,0.));
#4533=DIRECTION('ref_axis',(1.,0.,0.));
#4534=DIRECTION('',(0.,1.,0.));
#4535=DIRECTION('center_axis',(0.,1.,0.));
#4536=DIRECTION('ref_axis',(1.,0.,0.));
#4537=DIRECTION('center_axis',(0.,1.,0.));
#4538=DIRECTION('ref_axis',(-1.,0.,1.22464679914735E-16));
#4539=DIRECTION('center_axis',(0.157990501106673,0.987440631916705,0.));
#4540=DIRECTION('ref_axis',(0.987440631916706,-0.157990501106673,0.));
#4541=DIRECTION('center_axis',(-0.157990501106673,-0.987440631916705,0.));
#4542=DIRECTION('ref_axis',(0.987440631916705,-0.157990501106673,0.));
#4543=DIRECTION('',(0.,0.,1.));
#4544=DIRECTION('',(0.987440631916705,-0.157990501106673,0.));
#4545=DIRECTION('',(0.987440631916705,-0.157990501106673,0.));
#4546=DIRECTION('',(0.,0.,1.));
#4547=DIRECTION('',(0.987440631916705,-0.157990501106673,0.));
#4548=DIRECTION('center_axis',(1.,0.,0.));
#4549=DIRECTION('ref_axis',(0.,1.,0.));
#4550=DIRECTION('',(0.,1.,0.));
#4551=DIRECTION('center_axis',(-1.,0.,0.));
#4552=DIRECTION('ref_axis',(0.,-1.,0.));
#4553=DIRECTION('',(0.,-1.,0.));
#4554=DIRECTION('',(0.,-1.,0.));
#4555=DIRECTION('center_axis',(0.,0.,1.));
#4556=DIRECTION('ref_axis',(1.,0.,0.));
#4557=DIRECTION('',(0.,1.,0.));
#4558=DIRECTION('center_axis',(0.,1.,0.));
#4559=DIRECTION('ref_axis',(1.,0.,0.));
#4560=DIRECTION('center_axis',(0.,1.,0.));
#4561=DIRECTION('ref_axis',(1.,0.,0.));
#4562=DIRECTION('center_axis',(0.,1.,0.));
#4563=DIRECTION('ref_axis',(-1.,0.,1.22464679914735E-16));
#4564=DIRECTION('center_axis',(0.,1.,0.));
#4565=DIRECTION('ref_axis',(1.,0.,0.));
#4566=DIRECTION('center_axis',(0.,1.,0.));
#4567=DIRECTION('ref_axis',(1.,0.,0.));
#4568=DIRECTION('center_axis',(-0.157990501106673,0.987440631916705,0.));
#4569=DIRECTION('ref_axis',(-0.987440631916705,-0.157990501106673,0.));
#4570=DIRECTION('',(-0.987440631916705,-0.157990501106673,0.));
#4571=DIRECTION('center_axis',(0.157990501106673,-0.987440631916705,0.));
#4572=DIRECTION('ref_axis',(0.987440631916706,0.157990501106673,0.));
#4573=DIRECTION('',(0.,0.,1.));
#4574=DIRECTION('',(-0.987440631916705,-0.157990501106673,0.));
#4575=DIRECTION('',(-0.987440631916705,-0.157990501106673,0.));
#4576=DIRECTION('',(0.,0.,1.));
#4577=DIRECTION('center_axis',(0.,1.,0.));
#4578=DIRECTION('ref_axis',(1.,0.,0.));
#4579=DIRECTION('center_axis',(0.,1.,0.));
#4580=DIRECTION('ref_axis',(1.,0.,0.));
#4581=DIRECTION('center_axis',(0.,1.,0.));
#4582=DIRECTION('ref_axis',(1.,0.,0.));
#4583=DIRECTION('center_axis',(0.,1.,0.));
#4584=DIRECTION('ref_axis',(-1.,0.,-1.01064309961486E-15));
#4585=DIRECTION('center_axis',(0.,1.,0.));
#4586=DIRECTION('ref_axis',(1.,0.,0.));
#4587=DIRECTION('',(0.,-1.,0.));
#4588=DIRECTION('',(0.,1.,0.));
#4589=DIRECTION('center_axis',(0.,1.,0.));
#4590=DIRECTION('ref_axis',(1.,0.,0.));
#4591=DIRECTION('center_axis',(0.,1.,0.));
#4592=DIRECTION('ref_axis',(1.,0.,0.));
#4593=DIRECTION('center_axis',(1.,0.,0.));
#4594=DIRECTION('ref_axis',(0.,1.,0.));
#4595=DIRECTION('',(0.,1.,0.));
#4596=DIRECTION('center_axis',(-1.,0.,0.));
#4597=DIRECTION('ref_axis',(0.,-1.,0.));
#4598=DIRECTION('',(0.,-1.,0.));
#4599=DIRECTION('',(0.,-1.,0.));
#4600=DIRECTION('center_axis',(0.,0.,1.));
#4601=DIRECTION('ref_axis',(1.,0.,0.));
#4602=DIRECTION('',(0.,1.,0.));
#4603=DIRECTION('center_axis',(0.,0.,1.));
#4604=DIRECTION('ref_axis',(1.,0.,0.));
#4605=DIRECTION('center_axis',(0.,1.,0.));
#4606=DIRECTION('ref_axis',(1.,0.,0.));
#4607=DIRECTION('center_axis',(0.,1.,0.));
#4608=DIRECTION('ref_axis',(1.,0.,0.));
#4609=DIRECTION('center_axis',(0.,1.,0.));
#4610=DIRECTION('ref_axis',(1.,0.,0.));
#4611=DIRECTION('center_axis',(0.,1.,0.));
#4612=DIRECTION('ref_axis',(1.,0.,0.));
#4613=DIRECTION('center_axis',(0.,1.,0.));
#4614=DIRECTION('ref_axis',(-1.,0.,-1.22464679914735E-16));
#4615=DIRECTION('axis',(0.,0.,1.));
#4616=DIRECTION('refdir',(1.,0.,0.));
#4617=DIRECTION('center_axis',(0.,1.,0.));
#4618=DIRECTION('ref_axis',(1.,0.,0.));
#4619=DIRECTION('center_axis',(0.,-1.,0.));
#4620=DIRECTION('ref_axis',(1.,0.,0.));
#4621=DIRECTION('',(0.,-1.,0.));
#4622=DIRECTION('center_axis',(0.,-1.,0.));
#4623=DIRECTION('ref_axis',(1.,0.,0.));
#4624=DIRECTION('center_axis',(0.,1.,0.));
#4625=DIRECTION('ref_axis',(1.,0.,0.));
#4626=DIRECTION('center_axis',(0.,1.,0.));
#4627=DIRECTION('ref_axis',(1.,0.,0.));
#4628=DIRECTION('',(0.,-1.,0.));
#4629=DIRECTION('center_axis',(0.,1.,0.));
#4630=DIRECTION('ref_axis',(1.,0.,0.));
#4631=DIRECTION('center_axis',(0.,1.,0.));
#4632=DIRECTION('ref_axis',(1.,0.,0.));
#4633=DIRECTION('center_axis',(0.,1.,0.));
#4634=DIRECTION('ref_axis',(1.,0.,0.));
#4635=DIRECTION('axis',(0.,0.,1.));
#4636=DIRECTION('refdir',(1.,0.,0.));
#4637=DIRECTION('center_axis',(0.,1.,0.));
#4638=DIRECTION('ref_axis',(1.,0.,0.));
#4639=DIRECTION('center_axis',(0.,1.,0.));
#4640=DIRECTION('ref_axis',(1.,0.,0.));
#4641=DIRECTION('center_axis',(0.,1.,0.));
#4642=DIRECTION('ref_axis',(1.,0.,0.));
#4643=DIRECTION('center_axis',(0.,1.,0.));
#4644=DIRECTION('ref_axis',(1.,0.,0.));
#4645=DIRECTION('',(0.,-1.,0.));
#4646=DIRECTION('center_axis',(0.,1.,0.));
#4647=DIRECTION('ref_axis',(1.,0.,0.));
#4648=DIRECTION('center_axis',(0.,1.,0.));
#4649=DIRECTION('ref_axis',(1.,0.,0.));
#4650=DIRECTION('center_axis',(0.,-1.,0.));
#4651=DIRECTION('ref_axis',(1.,0.,0.));
#4652=DIRECTION('center_axis',(0.,1.,0.));
#4653=DIRECTION('ref_axis',(1.,0.,0.));
#4654=DIRECTION('',(0.,1.,0.));
#4655=DIRECTION('center_axis',(0.,-1.,0.));
#4656=DIRECTION('ref_axis',(1.,0.,0.));
#4657=DIRECTION('center_axis',(0.,1.,0.));
#4658=DIRECTION('ref_axis',(1.,0.,0.));
#4659=DIRECTION('',(-0.707106781186547,0.707106781186548,-8.65956056235493E-17));
#4660=DIRECTION('center_axis',(0.,-1.,0.));
#4661=DIRECTION('ref_axis',(1.,0.,0.));
#4662=DIRECTION('center_axis',(0.,1.,0.));
#4663=DIRECTION('ref_axis',(1.,0.,0.));
#4664=DIRECTION('',(-0.866025403784439,-0.5,-1.06057523872491E-16));
#4665=DIRECTION('center_axis',(1.92296268638356E-16,0.,-1.));
#4666=DIRECTION('ref_axis',(-1.,0.,-1.92296268638356E-16));
#4667=DIRECTION('',(0.,1.,0.));
#4668=DIRECTION('',(-1.,0.,-1.92296268638356E-16));
#4669=DIRECTION('',(0.,1.,0.));
#4670=DIRECTION('center_axis',(0.866025403784439,0.,-0.5));
#4671=DIRECTION('ref_axis',(-0.5,0.,-0.866025403784439));
#4672=DIRECTION('',(0.,1.,0.));
#4673=DIRECTION('',(-0.5,0.,-0.866025403784439));
#4674=DIRECTION('center_axis',(0.866025403784439,0.,0.5));
#4675=DIRECTION('ref_axis',(0.5,0.,-0.866025403784439));
#4676=DIRECTION('',(0.,1.,0.));
#4677=DIRECTION('',(0.5,0.,-0.866025403784439));
#4678=DIRECTION('center_axis',(-1.92296268638356E-16,0.,1.));
#4679=DIRECTION('ref_axis',(1.,0.,1.92296268638356E-16));
#4680=DIRECTION('',(0.,1.,0.));
#4681=DIRECTION('',(1.,0.,1.92296268638356E-16));
#4682=DIRECTION('center_axis',(-0.866025403784439,0.,0.5));
#4683=DIRECTION('ref_axis',(0.5,0.,0.866025403784439));
#4684=DIRECTION('',(0.,1.,0.));
#4685=DIRECTION('',(0.5,0.,0.866025403784439));
#4686=DIRECTION('center_axis',(-0.866025403784439,0.,-0.5));
#4687=DIRECTION('ref_axis',(-0.5,0.,0.866025403784439));
#4688=DIRECTION('',(-0.5,0.,0.866025403784438));
#4689=DIRECTION('center_axis',(0.,1.,0.));
#4690=DIRECTION('ref_axis',(0.,0.,1.));
#4691=DIRECTION('center_axis',(0.,1.,0.));
#4692=DIRECTION('ref_axis',(1.,0.,0.));
#4693=DIRECTION('axis',(0.,0.,1.));
#4694=DIRECTION('refdir',(1.,0.,0.));
#4695=DIRECTION('center_axis',(0.,1.,0.));
#4696=DIRECTION('ref_axis',(1.,0.,0.));
#4697=DIRECTION('center_axis',(0.,-1.,0.));
#4698=DIRECTION('ref_axis',(1.,0.,0.));
#4699=DIRECTION('',(0.,-1.,0.));
#4700=DIRECTION('center_axis',(0.,-1.,0.));
#4701=DIRECTION('ref_axis',(1.,0.,0.));
#4702=DIRECTION('center_axis',(0.,1.,0.));
#4703=DIRECTION('ref_axis',(1.,0.,0.));
#4704=DIRECTION('center_axis',(0.,1.,0.));
#4705=DIRECTION('ref_axis',(1.,0.,0.));
#4706=DIRECTION('',(0.,-1.,0.));
#4707=DIRECTION('center_axis',(0.,1.,0.));
#4708=DIRECTION('ref_axis',(1.,0.,0.));
#4709=DIRECTION('center_axis',(0.,1.,0.));
#4710=DIRECTION('ref_axis',(1.,0.,0.));
#4711=DIRECTION('center_axis',(0.,1.,0.));
#4712=DIRECTION('ref_axis',(1.,0.,0.));
#4713=DIRECTION('axis',(0.,0.,1.));
#4714=DIRECTION('refdir',(1.,0.,0.));
#4715=DIRECTION('center_axis',(0.,1.,0.));
#4716=DIRECTION('ref_axis',(1.,0.,0.));
#4717=DIRECTION('',(0.866025403784439,-0.5,1.06057523872491E-16));
#4718=DIRECTION('center_axis',(0.,-1.,0.));
#4719=DIRECTION('ref_axis',(1.,0.,0.));
#4720=DIRECTION('center_axis',(0.,-1.,0.));
#4721=DIRECTION('ref_axis',(1.,0.,0.));
#4722=DIRECTION('center_axis',(0.,1.,0.));
#4723=DIRECTION('ref_axis',(1.,0.,0.));
#4724=DIRECTION('',(-0.866025403784439,-0.5,-1.06057523872491E-16));
#4725=DIRECTION('center_axis',(1.92296268638356E-16,0.,-1.));
#4726=DIRECTION('ref_axis',(-1.,0.,-1.92296268638356E-16));
#4727=DIRECTION('',(0.,1.,0.));
#4728=DIRECTION('',(0.,1.,0.));
#4729=DIRECTION('center_axis',(-0.866025403784439,0.,-0.5));
#4730=DIRECTION('ref_axis',(-0.5,0.,0.866025403784439));
#4731=DIRECTION('',(0.,1.,0.));
#4732=DIRECTION('center_axis',(-0.866025403784439,0.,0.5));
#4733=DIRECTION('ref_axis',(0.5,0.,0.866025403784439));
#4734=DIRECTION('',(0.,1.,0.));
#4735=DIRECTION('center_axis',(0.,1.,0.));
#4736=DIRECTION('ref_axis',(1.,0.,0.));
#4737=DIRECTION('center_axis',(0.,1.,0.));
#4738=DIRECTION('ref_axis',(1.,0.,0.));
#4739=DIRECTION('',(0.,-1.,0.));
#4740=DIRECTION('center_axis',(0.,1.,0.));
#4741=DIRECTION('ref_axis',(1.,0.,0.));
#4742=DIRECTION('center_axis',(-1.92296268638356E-16,0.,1.));
#4743=DIRECTION('ref_axis',(1.,0.,1.92296268638356E-16));
#4744=DIRECTION('',(0.,1.,0.));
#4745=DIRECTION('center_axis',(0.866025403784439,0.,-0.5));
#4746=DIRECTION('ref_axis',(-0.5,0.,-0.866025403784439));
#4747=DIRECTION('',(0.,1.,0.));
#4748=DIRECTION('center_axis',(0.866025403784439,0.,0.5));
#4749=DIRECTION('ref_axis',(0.5,0.,-0.866025403784439));
#4750=DIRECTION('center_axis',(0.,1.,0.));
#4751=DIRECTION('ref_axis',(1.,0.,0.));
#4752=DIRECTION('center_axis',(0.,1.,0.));
#4753=DIRECTION('ref_axis',(1.,0.,0.));
#4754=DIRECTION('',(0.,0.,1.));
#4755=DIRECTION('',(1.,0.,0.));
#4756=DIRECTION('',(0.,0.,1.));
#4757=DIRECTION('',(1.,0.,0.));
#4758=DIRECTION('',(0.,0.,1.));
#4759=DIRECTION('',(1.,0.,0.));
#4760=DIRECTION('',(0.,0.,1.));
#4761=DIRECTION('',(1.,0.,0.));
#4762=DIRECTION('',(0.,0.,1.));
#4763=DIRECTION('',(1.,0.,0.));
#4764=DIRECTION('',(0.,0.,1.));
#4765=DIRECTION('',(1.,0.,0.));
#4766=DIRECTION('',(0.,0.,1.));
#4767=DIRECTION('',(1.,0.,0.));
#4768=DIRECTION('',(0.,0.,1.));
#4769=DIRECTION('',(1.,0.,0.));
#4770=DIRECTION('',(0.,0.,1.));
#4771=DIRECTION('',(1.,0.,0.));
#4772=DIRECTION('',(0.,0.,1.));
#4773=DIRECTION('',(1.,0.,0.));
#4774=DIRECTION('',(0.,0.,1.));
#4775=DIRECTION('',(1.,0.,0.));
#4776=DIRECTION('',(0.,0.,1.));
#4777=DIRECTION('',(1.,0.,0.));
#4778=DIRECTION('',(0.,0.,1.));
#4779=DIRECTION('',(1.,0.,0.));
#4780=DIRECTION('',(0.,0.,1.));
#4781=DIRECTION('',(1.,0.,0.));
#4782=DIRECTION('',(0.,0.,1.));
#4783=DIRECTION('',(1.,0.,0.));
#4784=DIRECTION('',(0.,0.,1.));
#4785=DIRECTION('',(1.,0.,0.));
#4786=DIRECTION('',(0.,0.,1.));
#4787=DIRECTION('',(1.,0.,0.));
#4788=DIRECTION('',(0.,0.,1.));
#4789=DIRECTION('',(1.,0.,0.));
#4790=DIRECTION('',(0.,0.,1.));
#4791=DIRECTION('',(1.,0.,0.));
#4792=DIRECTION('',(0.,0.,1.));
#4793=DIRECTION('',(1.,0.,0.));
#4794=DIRECTION('',(0.,0.,1.));
#4795=DIRECTION('',(1.,0.,0.));
#4796=DIRECTION('',(0.,0.,1.));
#4797=DIRECTION('',(1.,0.,0.));
#4798=DIRECTION('',(0.,0.,1.));
#4799=DIRECTION('',(1.,0.,0.));
#4800=DIRECTION('',(0.,0.,1.));
#4801=DIRECTION('',(1.,0.,0.));
#4802=DIRECTION('',(0.,0.,1.));
#4803=DIRECTION('',(1.,0.,0.));
#4804=DIRECTION('',(0.,0.,1.));
#4805=DIRECTION('',(1.,0.,0.));
#4806=DIRECTION('',(0.,0.,1.));
#4807=DIRECTION('',(1.,0.,0.));
#4808=DIRECTION('',(0.,0.,1.));
#4809=DIRECTION('',(1.,0.,0.));
#4810=DIRECTION('',(0.,0.,1.));
#4811=DIRECTION('',(1.,0.,0.));
#4812=DIRECTION('',(0.,0.,1.));
#4813=DIRECTION('',(1.,0.,0.));
#4814=DIRECTION('',(0.,0.,1.));
#4815=DIRECTION('',(1.,0.,0.));
#4816=DIRECTION('',(0.,0.,1.));
#4817=DIRECTION('',(1.,0.,0.));
#4818=DIRECTION('',(0.,0.,1.));
#4819=DIRECTION('',(1.,0.,0.));
#4820=DIRECTION('',(0.,0.,1.));
#4821=DIRECTION('',(1.,0.,0.));
#4822=DIRECTION('',(0.,0.,1.));
#4823=DIRECTION('',(1.,0.,0.));
#4824=DIRECTION('',(0.,0.,1.));
#4825=DIRECTION('',(1.,0.,0.));
#4826=DIRECTION('',(0.,0.,1.));
#4827=DIRECTION('',(1.,0.,0.));
#4828=DIRECTION('',(0.,0.,1.));
#4829=DIRECTION('',(1.,0.,0.));
#4830=DIRECTION('',(0.,0.,1.));
#4831=DIRECTION('',(1.,0.,0.));
#4832=DIRECTION('',(0.,0.,1.));
#4833=DIRECTION('',(1.,0.,0.));
#4834=DIRECTION('',(0.,0.,1.));
#4835=DIRECTION('',(1.,0.,0.));
#4836=DIRECTION('',(0.,0.,1.));
#4837=DIRECTION('',(1.,0.,0.));
#4838=DIRECTION('',(0.,0.,1.));
#4839=DIRECTION('',(1.,0.,0.));
#4840=DIRECTION('',(0.,0.,1.));
#4841=DIRECTION('',(1.,0.,0.));
#4842=DIRECTION('',(-0.629682207993501,1.09786644045143E-15,0.776852828363619));
#4843=DIRECTION('',(0.776852828363586,2.22769489030709E-15,0.629682207993475));
#4844=DIRECTION('',(-0.326007847973438,1.1496929078032E-15,0.945367062605761));
#4845=DIRECTION('',(0.945367062605724,1.82416841843144E-15,0.326007847973425));
#4846=DIRECTION('',(-0.189893181145098,1.34408111928537E-15,0.981804756433127));
#4847=DIRECTION('',(0.981804756433089,1.57418619744597E-15,0.18989318114509));
#4848=DIRECTION('',(-0.314579843307385,8.5655035708616E-16,0.949231016236204));
#4849=DIRECTION('',(0.949231016236167,2.44371416943161E-15,0.314579843307373));
#4850=DIRECTION('',(-0.0589949425730713,1.40003543065747E-15,0.998258281583918));
#4851=DIRECTION('',(0.998258281583892,2.07570050686326E-15,0.0589949425730699));
#4852=DIRECTION('',(0.242151194497772,1.88014775741807E-15,0.970238526859924));
#4853=DIRECTION('',(0.97023852685992,1.52147578801661E-15,-0.242151194497771));
#4854=DIRECTION('',(-0.603809875268449,5.49683868640875E-16,0.797128367660029));
#4855=DIRECTION('',(0.79712836766003,2.97282124886375E-16,0.603809875268449));
#4856=DIRECTION('',(-0.629682207993485,4.91306000786839E-16,0.776852828363578));
#4857=DIRECTION('',(0.776852828363579,2.14167211541235E-16,0.629682207993485));
#4858=CARTESIAN_POINT('',(0.,0.,0.));
#4859=CARTESIAN_POINT('',(0.,0.,0.));
#4860=CARTESIAN_POINT('',(0.,0.,0.));
#4861=CARTESIAN_POINT('Origin',(-1.5,-1.2,-0.1));
#4862=CARTESIAN_POINT('',(-1.775,-1.2,0.));
#4863=CARTESIAN_POINT('Origin',(-1.5,-1.2,0.));
#4864=CARTESIAN_POINT('',(-1.775,-1.2,0.5));
#4865=CARTESIAN_POINT('',(-1.775,-1.2,-0.1));
#4866=CARTESIAN_POINT('Origin',(-1.5,-1.2,0.5));
#4867=CARTESIAN_POINT('Origin',(-1.5,1.2,-0.1));
#4868=CARTESIAN_POINT('',(-1.775,1.2,0.));
#4869=CARTESIAN_POINT('Origin',(-1.5,1.2,0.));
#4870=CARTESIAN_POINT('',(-1.775,1.2,0.5));
#4871=CARTESIAN_POINT('',(-1.775,1.2,-0.1));
#4872=CARTESIAN_POINT('Origin',(-1.5,1.2,0.5));
#4873=CARTESIAN_POINT('Origin',(0.,-1.7,3.));
#4874=CARTESIAN_POINT('',(-0.41,-1.15,3.));
#4875=CARTESIAN_POINT('Origin',(0.,-1.15,3.));
#4876=CARTESIAN_POINT('',(-0.41,-0.85,3.));
#4877=CARTESIAN_POINT('',(-0.41,-1.7,3.));
#4878=CARTESIAN_POINT('Origin',(0.,-0.85,3.));
#4879=CARTESIAN_POINT('Origin',(0.,-1.7,3.));
#4880=CARTESIAN_POINT('',(-0.41,0.85,3.));
#4881=CARTESIAN_POINT('Origin',(0.,0.85,3.));
#4882=CARTESIAN_POINT('',(-0.41,1.15,3.));
#4883=CARTESIAN_POINT('',(-0.41,-1.7,3.));
#4884=CARTESIAN_POINT('Origin',(0.,1.15,3.));
#4885=CARTESIAN_POINT('Origin',(0.,0.85,3.));
#4886=CARTESIAN_POINT('',(-0.4,0.85,2.4255437353462));
#4887=CARTESIAN_POINT('',(-0.4,1.15,2.4255437353462));
#4888=CARTESIAN_POINT('',(-0.4,0.85,2.4255437353462));
#4889=CARTESIAN_POINT('',(0.4,0.85,2.4255437353462));
#4890=CARTESIAN_POINT('Origin',(0.,0.85,3.));
#4891=CARTESIAN_POINT('',(0.4,1.15,2.4255437353462));
#4892=CARTESIAN_POINT('',(0.4,0.85,2.4255437353462));
#4893=CARTESIAN_POINT('Origin',(0.,1.15,3.));
#4894=CARTESIAN_POINT('Origin',(0.,1.15,1.7));
#4895=CARTESIAN_POINT('',(0.4,1.15,0.4));
#4896=CARTESIAN_POINT('',(0.4,1.15,0.4));
#4897=CARTESIAN_POINT('',(0.,1.15,0.4));
#4898=CARTESIAN_POINT('',(-0.4,1.15,0.4));
#4899=CARTESIAN_POINT('',(0.,1.15,0.5));
#4900=CARTESIAN_POINT('',(0.,1.15,0.85));
#4901=CARTESIAN_POINT('',(-0.4,1.15,0.5));
#4902=CARTESIAN_POINT('',(-0.75,1.15,0.5));
#4903=CARTESIAN_POINT('',(-0.4,1.15,3.));
#4904=CARTESIAN_POINT('Origin',(0.4,0.85,3.));
#4905=CARTESIAN_POINT('',(0.4,0.85,0.4));
#4906=CARTESIAN_POINT('',(0.4,0.85,0.4));
#4907=CARTESIAN_POINT('',(0.4,0.85,0.4));
#4908=CARTESIAN_POINT('Origin',(0.,0.85,1.7));
#4909=CARTESIAN_POINT('',(-0.4,0.85,0.5));
#4910=CARTESIAN_POINT('',(-0.4,0.85,3.));
#4911=CARTESIAN_POINT('',(0.,0.85,0.5));
#4912=CARTESIAN_POINT('',(-0.75,0.85,0.5));
#4913=CARTESIAN_POINT('',(0.,0.85,0.4));
#4914=CARTESIAN_POINT('',(0.,0.85,0.85));
#4915=CARTESIAN_POINT('',(-0.4,0.85,0.4));
#4916=CARTESIAN_POINT('Origin',(0.4,0.85,0.4));
#4917=CARTESIAN_POINT('',(0.,-0.575,0.4));
#4918=CARTESIAN_POINT('Origin',(-0.4,0.85,0.4));
#4919=CARTESIAN_POINT('',(-0.4,0.425,0.5));
#4920=CARTESIAN_POINT('Origin',(-1.5,0.,0.5));
#4921=CARTESIAN_POINT('',(0.,2.,0.5));
#4922=CARTESIAN_POINT('',(0.,-2.,0.5));
#4923=CARTESIAN_POINT('',(-3.,2.,0.5));
#4924=CARTESIAN_POINT('',(0.,2.,0.5));
#4925=CARTESIAN_POINT('',(-3.,-2.,0.5));
#4926=CARTESIAN_POINT('',(-3.,2.,0.5));
#4927=CARTESIAN_POINT('',(0.,-2.,0.5));
#4928=CARTESIAN_POINT('',(-3.,-2.,0.5));
#4929=CARTESIAN_POINT('',(0.,-1.15,0.5));
#4930=CARTESIAN_POINT('',(0.,-2.,0.5));
#4931=CARTESIAN_POINT('',(-0.4,-1.15,0.5));
#4932=CARTESIAN_POINT('',(-0.75,-1.15,0.5));
#4933=CARTESIAN_POINT('',(-0.4,-0.85,0.5));
#4934=CARTESIAN_POINT('',(-0.4,-0.575,0.5));
#4935=CARTESIAN_POINT('',(0.,-0.85,0.5));
#4936=CARTESIAN_POINT('',(-0.75,-0.85,0.5));
#4937=CARTESIAN_POINT('',(0.,-2.,0.5));
#4938=CARTESIAN_POINT('Origin',(0.,-1.15,3.));
#4939=CARTESIAN_POINT('',(-0.4,-1.15,2.4255437353462));
#4940=CARTESIAN_POINT('',(-0.4,-0.85,2.4255437353462));
#4941=CARTESIAN_POINT('',(-0.4,-1.15,2.4255437353462));
#4942=CARTESIAN_POINT('',(0.4,-1.15,2.4255437353462));
#4943=CARTESIAN_POINT('Origin',(0.,-1.15,3.));
#4944=CARTESIAN_POINT('',(0.4,-0.85,2.4255437353462));
#4945=CARTESIAN_POINT('',(0.4,-1.15,2.4255437353462));
#4946=CARTESIAN_POINT('Origin',(0.,-0.85,3.));
#4947=CARTESIAN_POINT('Origin',(0.,-0.85,1.7));
#4948=CARTESIAN_POINT('',(0.4,-0.85,0.4));
#4949=CARTESIAN_POINT('',(0.4,-0.85,0.4));
#4950=CARTESIAN_POINT('',(0.,-0.85,0.4));
#4951=CARTESIAN_POINT('',(-0.4,-0.85,0.4));
#4952=CARTESIAN_POINT('',(0.,-0.85,0.85));
#4953=CARTESIAN_POINT('',(-0.4,-0.85,3.));
#4954=CARTESIAN_POINT('Origin',(0.4,-1.15,3.));
#4955=CARTESIAN_POINT('',(0.4,-1.15,0.4));
#4956=CARTESIAN_POINT('',(0.4,-1.15,0.4));
#4957=CARTESIAN_POINT('',(0.4,-1.15,0.4));
#4958=CARTESIAN_POINT('Origin',(0.,-1.15,1.7));
#4959=CARTESIAN_POINT('',(-0.4,-1.15,3.));
#4960=CARTESIAN_POINT('',(0.,-1.15,0.4));
#4961=CARTESIAN_POINT('',(0.,-1.15,0.85));
#4962=CARTESIAN_POINT('',(-0.4,-1.15,0.4));
#4963=CARTESIAN_POINT('Origin',(0.4,-1.15,0.4));
#4964=CARTESIAN_POINT('',(0.,-1.575,0.4));
#4965=CARTESIAN_POINT('Origin',(-0.4,-1.15,0.4));
#4966=CARTESIAN_POINT('Origin',(0.,2.,0.));
#4967=CARTESIAN_POINT('',(0.,2.,0.));
#4968=CARTESIAN_POINT('',(-3.,2.,0.));
#4969=CARTESIAN_POINT('',(0.,2.,0.));
#4970=CARTESIAN_POINT('',(-3.,2.,0.));
#4971=CARTESIAN_POINT('',(0.,2.,0.));
#4972=CARTESIAN_POINT('Origin',(0.,-2.,0.));
#4973=CARTESIAN_POINT('',(0.,-2.,0.));
#4974=CARTESIAN_POINT('',(0.,-2.,0.));
#4975=CARTESIAN_POINT('',(0.,-2.,0.));
#4976=CARTESIAN_POINT('Origin',(-3.,-2.,0.));
#4977=CARTESIAN_POINT('',(-3.,-2.,0.));
#4978=CARTESIAN_POINT('',(-3.,-2.,0.));
#4979=CARTESIAN_POINT('',(-3.,-2.,0.));
#4980=CARTESIAN_POINT('Origin',(-3.,2.,0.));
#4981=CARTESIAN_POINT('',(-3.,2.,0.));
#4982=CARTESIAN_POINT('Origin',(-1.5,0.,0.));
#4983=CARTESIAN_POINT('',(0.,0.,0.));
#4984=CARTESIAN_POINT('',(0.,0.,0.));
#4985=CARTESIAN_POINT('Origin',(-8.88178419700125E-16,-1.70000000000019,
3.));
#4986=CARTESIAN_POINT('',(-0.385273960864878,-1.52000000000017,2.8597717037131));
#4987=CARTESIAN_POINT('Origin',(-8.88178419700125E-16,-1.52000000000017,
3.));
#4988=CARTESIAN_POINT('',(-0.385273960864878,-1.28000000000015,2.8597717037131));
#4989=CARTESIAN_POINT('',(-0.385273960864878,-1.70000000000019,2.8597717037131));
#4990=CARTESIAN_POINT('',(-0.140228296286904,-1.28000000000015,3.38527396086488));
#4991=CARTESIAN_POINT('Origin',(-8.88178419700125E-16,-1.28000000000015,
3.));
#4992=CARTESIAN_POINT('',(0.140228296286902,-1.28000000000015,2.61472603913512));
#4993=CARTESIAN_POINT('Origin',(-8.88178419700125E-16,-1.28000000000015,
3.));
#4994=CARTESIAN_POINT('Origin',(-8.88178419700125E-16,-1.28000000000015,
3.));
#4995=CARTESIAN_POINT('Origin',(-8.88178419700125E-16,-1.70000000000019,
3.));
#4996=CARTESIAN_POINT('',(-0.140228296286904,1.28000000000015,3.38527396086488));
#4997=CARTESIAN_POINT('',(0.140228296286902,1.28000000000015,2.61472603913512));
#4998=CARTESIAN_POINT('Origin',(-8.88178419700125E-16,1.28000000000015,
3.));
#4999=CARTESIAN_POINT('',(-0.385273960864878,1.28000000000015,2.8597717037131));
#5000=CARTESIAN_POINT('Origin',(-8.88178419700125E-16,1.28000000000015,
3.));
#5001=CARTESIAN_POINT('',(-0.385273960864878,1.52000000000017,2.8597717037131));
#5002=CARTESIAN_POINT('',(-0.385273960864878,-1.70000000000019,2.8597717037131));
#5003=CARTESIAN_POINT('Origin',(-8.88178419700125E-16,1.52000000000017,
3.));
#5004=CARTESIAN_POINT('Origin',(-8.88178419700125E-16,1.28000000000015,
3.));
#5005=CARTESIAN_POINT('Origin',(2.34923146868827,-1.70000000000019,3.85505058711526));
#5006=CARTESIAN_POINT('',(2.20900317240137,-1.12000000000013,4.24032454798014));
#5007=CARTESIAN_POINT('',(2.48945976497518,-1.12000000000013,3.46977662625038));
#5008=CARTESIAN_POINT('Origin',(2.34923146868827,-1.12000000000013,3.85505058711526));
#5009=CARTESIAN_POINT('',(1.9639575078234,-1.18560000000013,3.71482229082836));
#5010=CARTESIAN_POINT('Origin',(2.34923146868827,-1.12000000000013,3.85505058711526));
#5011=CARTESIAN_POINT('',(1.9639575078234,-0.8800000000001,3.71482229082836));
#5012=CARTESIAN_POINT('',(1.9639575078234,-1.70000000000019,3.71482229082836));
#5013=CARTESIAN_POINT('Origin',(2.34923146868827,-0.8800000000001,3.85505058711526));
#5014=CARTESIAN_POINT('Origin',(2.34923146868827,-1.12000000000013,3.85505058711526));
#5015=CARTESIAN_POINT('Origin',(2.34923146868827,-1.70000000000019,3.85505058711526));
#5016=CARTESIAN_POINT('',(1.9639575078234,0.8800000000001,3.71482229082836));
#5017=CARTESIAN_POINT('Origin',(2.34923146868827,0.8800000000001,3.85505058711526));
#5018=CARTESIAN_POINT('',(1.9639575078234,1.18560000000014,3.71482229082836));
#5019=CARTESIAN_POINT('',(1.9639575078234,-1.70000000000019,3.71482229082836));
#5020=CARTESIAN_POINT('',(2.20900317240137,1.12000000000013,4.24032454798014));
#5021=CARTESIAN_POINT('Origin',(2.34923146868827,1.12000000000013,3.85505058711526));
#5022=CARTESIAN_POINT('',(2.48945976497518,1.12000000000013,3.46977662625038));
#5023=CARTESIAN_POINT('Origin',(2.34923146868827,1.12000000000013,3.85505058711526));
#5024=CARTESIAN_POINT('Origin',(2.34923146868827,1.12000000000013,3.85505058711526));
#5025=CARTESIAN_POINT('Origin',(-8.88178419700125E-16,1.28000000000015,
3.));
#5026=CARTESIAN_POINT('',(-0.239414164392274,1.28000000000015,3.65778481123272));
#5027=CARTESIAN_POINT('',(0.342020234846104,1.28000000000015,2.06030741252469));
#5028=CARTESIAN_POINT('',(0.239414164392272,1.28000000000015,2.34221518876728));
#5029=CARTESIAN_POINT('Origin',(-8.88178419700125E-16,1.28000000000015,
3.));
#5030=CARTESIAN_POINT('',(0.342020234846104,1.28000000000015,2.06030741252469));
#5031=CARTESIAN_POINT('Origin',(-8.88178419700125E-16,-1.28000000000015,
3.));
#5032=CARTESIAN_POINT('',(0.239414164392273,-1.28000000000015,2.34221518876728));
#5033=CARTESIAN_POINT('',(0.342020234846104,-1.28000000000015,2.06030741252469));
#5034=CARTESIAN_POINT('',(-0.239414164392274,-1.28000000000015,3.65778481123272));
#5035=CARTESIAN_POINT('Origin',(-8.88178419700125E-16,-1.28000000000015,
3.));
#5036=CARTESIAN_POINT('',(0.342020234846104,-1.28000000000015,2.06030741252469));
#5037=CARTESIAN_POINT('Origin',(3.03327193838048,1.12000000000013,1.97566541216464));
#5038=CARTESIAN_POINT('',(2.58864563308055,1.12000000000013,3.19726577588254));
#5039=CARTESIAN_POINT('',(3.03327193838048,1.12000000000013,1.97566541216464));
#5040=CARTESIAN_POINT('',(3.03327193838048,1.12000000000013,1.97566541216464));
#5041=CARTESIAN_POINT('',(3.03327193838048,1.12000000000013,1.97566541216464));
#5042=CARTESIAN_POINT('',(0.684040469692209,1.52000000000017,1.12061482504938));
#5043=CARTESIAN_POINT('',(3.03327193838048,1.12000000000013,1.97566541216464));
#5044=CARTESIAN_POINT('',(0.239414164392272,1.52000000000017,2.34221518876728));
#5045=CARTESIAN_POINT('',(0.684040469692209,1.52000000000017,1.12061482504938));
#5046=CARTESIAN_POINT('',(-0.239414164392274,1.52000000000017,3.65778481123272));
#5047=CARTESIAN_POINT('Origin',(-8.88178419700125E-16,1.52000000000017,
3.));
#5048=CARTESIAN_POINT('',(2.109817304296,1.12000000000013,4.51283539834798));
#5049=CARTESIAN_POINT('',(2.109817304296,1.12000000000013,4.51283539834798));
#5050=CARTESIAN_POINT('',(3.03327193838048,1.12000000000013,1.97566541216464));
#5051=CARTESIAN_POINT('Origin',(0.684040469692209,-1.52000000000017,1.12061482504938));
#5052=CARTESIAN_POINT('',(2.109817304296,-1.12000000000013,4.51283539834798));
#5053=CARTESIAN_POINT('',(3.03327193838048,-1.12000000000013,1.97566541216464));
#5054=CARTESIAN_POINT('',(-0.239414164392274,-1.52000000000017,3.65778481123272));
#5055=CARTESIAN_POINT('',(-0.239414164392274,-1.52000000000017,3.65778481123272));
#5056=CARTESIAN_POINT('',(0.239414164392273,-1.52000000000017,2.34221518876728));
#5057=CARTESIAN_POINT('Origin',(-8.88178419700125E-16,-1.52000000000017,
3.));
#5058=CARTESIAN_POINT('',(0.684040469692209,-1.52000000000017,1.12061482504938));
#5059=CARTESIAN_POINT('',(0.684040469692209,-1.52000000000017,1.12061482504938));
#5060=CARTESIAN_POINT('',(3.03327193838048,-1.12000000000013,1.97566541216464));
#5061=CARTESIAN_POINT('',(0.684040469692209,-1.52000000000017,1.12061482504938));
#5062=CARTESIAN_POINT('',(2.58864563308055,-1.12000000000013,3.19726577588255));
#5063=CARTESIAN_POINT('',(3.03327193838048,-1.12000000000013,1.97566541216464));
#5064=CARTESIAN_POINT('',(3.03327193838048,-1.12000000000013,1.97566541216464));
#5065=CARTESIAN_POINT('Origin',(1.43579453967246,1.30000000000015,1.39423101292626));
#5066=CARTESIAN_POINT('',(1.33318846921863,-1.15200000000013,1.67613878916886));
#5067=CARTESIAN_POINT('',(1.43579453967246,-1.15200000000013,1.39423101292626));
#5068=CARTESIAN_POINT('',(1.43579453967246,-1.15200000000013,1.39423101292626));
#5069=CARTESIAN_POINT('',(1.33318846921863,1.15200000000013,1.67613878916886));
#5070=CARTESIAN_POINT('',(1.33318846921863,1.30000000000015,1.67613878916886));
#5071=CARTESIAN_POINT('',(1.43579453967246,1.15200000000013,1.39423101292626));
#5072=CARTESIAN_POINT('',(1.43579453967246,1.15200000000013,1.39423101292626));
#5073=CARTESIAN_POINT('',(1.43579453967246,1.30000000000015,1.39423101292626));
#5074=CARTESIAN_POINT('Origin',(2.28151786840024,-1.15000000000013,1.70204922428776));
#5075=CARTESIAN_POINT('',(2.28151786840024,-1.00800000000012,1.70204922428776));
#5076=CARTESIAN_POINT('',(2.17891179794641,-1.00800000000012,1.98395700053035));
#5077=CARTESIAN_POINT('',(2.28151786840024,-1.00800000000012,1.70204922428776));
#5078=CARTESIAN_POINT('',(2.28151786840024,1.00800000000012,1.70204922428776));
#5079=CARTESIAN_POINT('',(2.28151786840024,-1.15000000000013,1.70204922428776));
#5080=CARTESIAN_POINT('',(2.17891179794641,1.00800000000012,1.98395700053035));
#5081=CARTESIAN_POINT('',(2.28151786840024,1.00800000000012,1.70204922428776));
#5082=CARTESIAN_POINT('',(2.17891179794641,-1.15000000000013,1.98395700053035));
#5083=CARTESIAN_POINT('Origin',(1.75605013358252,1.07527058761815E-16,1.8300478948496));
#5084=CARTESIAN_POINT('',(2.42252087083831,-0.966521060842544,2.07262347872934));
#5085=CARTESIAN_POINT('',(1.24790513649417,1.16652106084257,1.64509818517171));
#5086=CARTESIAN_POINT('Origin',(2.34923146868827,0.880000000000101,3.85505058711526));
#5087=CARTESIAN_POINT('',(2.58864563308055,0.880000000000101,3.19726577588255));
#5088=CARTESIAN_POINT('',(2.109817304296,0.880000000000101,4.51283539834798));
#5089=CARTESIAN_POINT('Origin',(2.34923146868827,0.880000000000101,3.85505058711526));
#5090=CARTESIAN_POINT('Origin',(2.34923146868827,0.880000000000101,3.85505058711526));
#5091=CARTESIAN_POINT('Origin',(2.34923146868827,0.880000000000101,3.85505058711526));
#5092=CARTESIAN_POINT('',(2.58864563308055,0.880000000000101,3.19726577588255));
#5093=CARTESIAN_POINT('Origin',(2.34923146868827,1.12000000000013,3.85505058711526));
#5094=CARTESIAN_POINT('',(2.109817304296,0.880000000000101,4.51283539834798));
#5095=CARTESIAN_POINT('Origin',(2.34923146868827,1.12000000000013,3.85505058711526));
#5096=CARTESIAN_POINT('Origin',(2.34923146868827,0.880000000000101,3.85505058711526));
#5097=CARTESIAN_POINT('Origin',(2.34923146868827,0.880000000000101,3.85505058711526));
#5098=CARTESIAN_POINT('Origin',(0.684040469692209,1.28000000000015,1.12061482504938));
#5099=CARTESIAN_POINT('',(0.684040469692209,1.28000000000015,1.12061482504938));
#5100=CARTESIAN_POINT('',(0.684040469692209,1.28000000000015,1.12061482504938));
#5101=CARTESIAN_POINT('',(0.684040469692209,1.28000000000015,1.12061482504938));
#5102=CARTESIAN_POINT('',(3.03327193838048,0.880000000000101,1.97566541216464));
#5103=CARTESIAN_POINT('',(0.684040469692209,1.28000000000015,1.12061482504938));
#5104=CARTESIAN_POINT('',(3.03327193838048,0.880000000000101,1.97566541216464));
#5105=CARTESIAN_POINT('',(-0.239414164392274,1.28000000000015,3.65778481123272));
#5106=CARTESIAN_POINT('Origin',(3.03327193838048,0.880000000000101,1.97566541216464));
#5107=CARTESIAN_POINT('',(3.03327193838048,0.880000000000101,1.97566541216464));
#5108=CARTESIAN_POINT('Origin',(0.684040469692209,1.52000000000017,1.12061482504938));
#5109=CARTESIAN_POINT('',(0.239414164392272,1.28000000000015,2.34221518876728));
#5110=CARTESIAN_POINT('',(0.684040469692209,1.52000000000017,1.12061482504938));
#5111=CARTESIAN_POINT('Origin',(0.935201569951863,1.20000000000014,4.08531010479035));
#5112=CARTESIAN_POINT('',(-0.239414164392274,1.28000000000015,3.65778481123272));
#5113=CARTESIAN_POINT('Origin',(-8.88178419700125E-16,1.28000000000015,
3.));
#5114=CARTESIAN_POINT('Origin',(-8.88178419700125E-16,1.52000000000017,
3.));
#5115=CARTESIAN_POINT('Origin',(-8.88178419700125E-16,1.28000000000015,
3.));
#5116=CARTESIAN_POINT('Origin',(-8.88178419700125E-16,1.52000000000017,
3.));
#5117=CARTESIAN_POINT('Origin',(-8.88178419700125E-16,1.52000000000017,
3.));
#5118=CARTESIAN_POINT('Origin',(3.03327193838048,-0.8800000000001,1.97566541216464));
#5119=CARTESIAN_POINT('',(2.109817304296,-0.8800000000001,4.51283539834798));
#5120=CARTESIAN_POINT('',(2.109817304296,-0.8800000000001,4.51283539834798));
#5121=CARTESIAN_POINT('',(2.58864563308055,-0.8800000000001,3.19726577588255));
#5122=CARTESIAN_POINT('Origin',(2.34923146868827,-0.8800000000001,3.85505058711526));
#5123=CARTESIAN_POINT('',(3.03327193838048,-0.8800000000001,1.97566541216464));
#5124=CARTESIAN_POINT('',(3.03327193838048,-0.8800000000001,1.97566541216464));
#5125=CARTESIAN_POINT('',(3.03327193838048,-0.8800000000001,1.97566541216464));
#5126=CARTESIAN_POINT('',(0.684040469692209,-1.28000000000015,1.12061482504938));
#5127=CARTESIAN_POINT('',(3.03327193838048,-0.8800000000001,1.97566541216464));
#5128=CARTESIAN_POINT('',(0.684040469692209,-1.28000000000015,1.12061482504938));
#5129=CARTESIAN_POINT('Origin',(2.34923146868827,-0.8800000000001,3.85505058711526));
#5130=CARTESIAN_POINT('Origin',(2.34923146868827,-0.8800000000001,3.85505058711526));
#5131=CARTESIAN_POINT('Origin',(2.34923146868827,-0.8800000000001,3.85505058711526));
#5132=CARTESIAN_POINT('Origin',(2.34923146868827,-1.12000000000013,3.85505058711526));
#5133=CARTESIAN_POINT('Origin',(2.34923146868827,-1.12000000000013,3.85505058711526));
#5134=CARTESIAN_POINT('',(2.58864563308055,-1.12000000000013,3.19726577588255));
#5135=CARTESIAN_POINT('',(2.109817304296,-1.12000000000013,4.51283539834798));
#5136=CARTESIAN_POINT('Origin',(2.34923146868827,-1.12000000000013,3.85505058711526));
#5137=CARTESIAN_POINT('Origin',(2.34923146868827,-1.12000000000013,3.85505058711526));
#5138=CARTESIAN_POINT('Origin',(3.03327193838048,-1.12000000000013,1.97566541216464));
#5139=CARTESIAN_POINT('',(3.03327193838048,-1.12000000000013,1.97566541216464));
#5140=CARTESIAN_POINT('Origin',(0.684040469692209,-1.28000000000015,1.12061482504938));
#5141=CARTESIAN_POINT('',(0.239414164392273,-1.52000000000017,2.34221518876728));
#5142=CARTESIAN_POINT('',(0.684040469692209,-1.28000000000015,1.12061482504938));
#5143=CARTESIAN_POINT('Origin',(0.935201569951863,-1.20000000000014,4.08531010479035));
#5144=CARTESIAN_POINT('',(-0.239414164392274,-1.52000000000017,3.65778481123272));
#5145=CARTESIAN_POINT('Origin',(1.85865620403635,-1.20000000000014,1.54814011860701));
#5146=CARTESIAN_POINT('Origin',(-8.88178419700125E-16,-1.52000000000017,
3.));
#5147=CARTESIAN_POINT('Origin',(-8.88178419700125E-16,-1.52000000000017,
3.));
#5148=CARTESIAN_POINT('Origin',(-8.88178419700125E-16,-1.52000000000017,
3.));
#5149=CARTESIAN_POINT('Origin',(-8.88178419700125E-16,-1.52000000000017,
3.));
#5150=CARTESIAN_POINT('Origin',(-8.88178419700125E-16,-1.52000000000017,
3.));
#5151=CARTESIAN_POINT('',(0.,0.,0.));
#5152=CARTESIAN_POINT('Origin',(2.34923146868827,-1.56000000000018,3.85505058711526));
#5153=CARTESIAN_POINT('',(2.05792676657093,1.56000000000018,3.74902431431297));
#5154=CARTESIAN_POINT('Origin',(2.34923146868827,1.56000000000018,3.85505058711526));
#5155=CARTESIAN_POINT('',(2.05792676657093,-1.56000000000018,3.74902431431297));
#5156=CARTESIAN_POINT('',(2.05792676657093,-1.56000000000018,3.74902431431297));
#5157=CARTESIAN_POINT('Origin',(2.34923146868827,-1.56000000000018,3.85505058711526));
#5158=CARTESIAN_POINT('Origin',(2.34923146868827,-1.56000000000018,3.85505058711526));
#5159=CARTESIAN_POINT('',(1.97335443369815,1.56000000000018,3.71824249317682));
#5160=CARTESIAN_POINT('Origin',(2.34923146868827,1.56000000000018,3.85505058711526));
#5161=CARTESIAN_POINT('',(1.97335443369815,-1.56000000000018,3.71824249317682));
#5162=CARTESIAN_POINT('',(1.97335443369815,-1.56000000000018,3.71824249317682));
#5163=CARTESIAN_POINT('Origin',(2.34923146868827,-1.56000000000018,3.85505058711526));
#5164=CARTESIAN_POINT('Origin',(2.34923146868827,1.56000000000018,3.85505058711526));
#5165=CARTESIAN_POINT('Origin',(2.34923146868827,-1.56000000000018,3.85505058711526));
#5166=CARTESIAN_POINT('',(0.,0.,0.));
#5167=CARTESIAN_POINT('Origin',(2.34923146868827,-1.27000000000034,3.85505058711526));
#5168=CARTESIAN_POINT('',(2.06732369244568,-1.27000000000034,3.75244451666143));
#5169=CARTESIAN_POINT('Origin',(2.34923146868827,-1.27000000000034,3.85505058711526));
#5170=CARTESIAN_POINT('',(2.11430832181945,-1.27000000000034,3.76954552840374));
#5171=CARTESIAN_POINT('Origin',(2.34923146868827,-1.27000000000034,3.85505058711526));
#5172=CARTESIAN_POINT('Origin',(2.34923146868828,-2.28000000000046,3.85505058711526));
#5173=CARTESIAN_POINT('',(2.06732369244568,-2.28000000000046,3.75244451666143));
#5174=CARTESIAN_POINT('',(2.06732369244568,-2.28000000000046,3.75244451666143));
#5175=CARTESIAN_POINT('Origin',(2.34923146868828,-2.28000000000046,3.85505058711526));
#5176=CARTESIAN_POINT('Origin',(2.34923146868828,-2.28000000000046,3.85505058711526));
#5177=CARTESIAN_POINT('Origin',(2.34923146868827,0.274999999999834,3.85505058711526));
#5178=CARTESIAN_POINT('',(2.07277390945304,-1.22580000000034,3.75442823402354));
#5179=CARTESIAN_POINT('Origin',(2.34923146868827,-1.22580000000034,3.85505058711526));
#5180=CARTESIAN_POINT('',(2.07277390945304,1.72,3.75442823402354));
#5181=CARTESIAN_POINT('',(2.07277390945304,0.274999999999834,3.75442823402354));
#5182=CARTESIAN_POINT('Origin',(2.34923146868827,1.72,3.85505058711526));
#5183=CARTESIAN_POINT('Origin',(2.34923146868827,-1.25000000000034,3.85505058711526));
#5184=CARTESIAN_POINT('',(2.09551447006994,-1.25000000000034,3.76270512370681));
#5185=CARTESIAN_POINT('Origin',(2.34923146868827,2.06158650880643,3.85505058711526));
#5186=CARTESIAN_POINT('',(1.9028774896375,2.12000000000004,3.69259097556336));
#5187=CARTESIAN_POINT('Origin',(2.34923146868827,2.12000000000004,3.85505058711526));
#5188=CARTESIAN_POINT('',(1.80669970035391,2.06090804453178,3.65758511245857));
#5189=CARTESIAN_POINT('',(1.80780396562194,2.06158650880643,3.65798703226866));
#5190=CARTESIAN_POINT('',(1.90695546709804,2.06090804453178,4.22616414352457));
#5191=CARTESIAN_POINT('Ctrl Pts',(1.90695546709804,2.06090804453178,4.22616414352457));
#5192=CARTESIAN_POINT('Ctrl Pts',(1.8568275837256,2.14424137786374,3.94187462798943));
#5193=CARTESIAN_POINT('Ctrl Pts',(1.80669970035391,2.06090804453178,3.65758511245857));
#5194=CARTESIAN_POINT('',(2.44948723543241,2.06090804453178,4.42362961818127));
#5195=CARTESIAN_POINT('Ctrl Pts',(2.44948723543241,2.06090804453178,4.42362961818127));
#5196=CARTESIAN_POINT('Ctrl Pts',(2.17822135126319,2.14424137786374,4.32489688085218));
#5197=CARTESIAN_POINT('Ctrl Pts',(1.90695546709804,2.06090804453178,4.22616414352457));
#5198=CARTESIAN_POINT('',(2.89176323702264,2.06090804453178,4.05251606177196));
#5199=CARTESIAN_POINT('Ctrl Pts',(2.89176323702264,2.06090804453178,4.05251606177196));
#5200=CARTESIAN_POINT('Ctrl Pts',(2.67062523622586,2.14424137786374,4.23807283997801));
#5201=CARTESIAN_POINT('Ctrl Pts',(2.44948723543241,2.06090804453178,4.42362961818127));
#5202=CARTESIAN_POINT('',(2.79150747027851,2.06090804453178,3.48393703070596));
#5203=CARTESIAN_POINT('Ctrl Pts',(2.79150747027851,2.06090804453178,3.48393703070596));
#5204=CARTESIAN_POINT('Ctrl Pts',(2.84163535365095,2.14424137786374,3.76822654624109));
#5205=CARTESIAN_POINT('Ctrl Pts',(2.89176323702264,2.06090804453178,4.05251606177196));
#5206=CARTESIAN_POINT('',(2.24897570194414,2.06090804453178,3.28647155604926));
#5207=CARTESIAN_POINT('Ctrl Pts',(2.24897570194414,2.06090804453178,3.28647155604926));
#5208=CARTESIAN_POINT('Ctrl Pts',(2.52024158611336,2.14424137786374,3.38520429337835));
#5209=CARTESIAN_POINT('Ctrl Pts',(2.79150747027851,2.06090804453178,3.48393703070596));
#5210=CARTESIAN_POINT('Ctrl Pts',(1.80669970035391,2.06090804453178,3.65758511245857));
#5211=CARTESIAN_POINT('Ctrl Pts',(2.02783770115069,2.14424137786374,3.47202833425252));
#5212=CARTESIAN_POINT('Ctrl Pts',(2.24897570194414,2.06090804453178,3.28647155604926));
#5213=CARTESIAN_POINT('Origin',(2.79150747027851,1.72,3.48393703070596));
#5214=CARTESIAN_POINT('',(2.79150747027851,1.72,3.48393703070596));
#5215=CARTESIAN_POINT('',(2.79150747027851,1.72,3.48393703070596));
#5216=CARTESIAN_POINT('',(2.24897570194414,1.72,3.28647155604926));
#5217=CARTESIAN_POINT('',(2.79150747027851,1.72,3.48393703070596));
#5218=CARTESIAN_POINT('',(2.24897570194414,1.72,3.28647155604926));
#5219=CARTESIAN_POINT('Origin',(2.89176323702264,1.72,4.05251606177196));
#5220=CARTESIAN_POINT('',(2.89176323702264,1.72,4.05251606177196));
#5221=CARTESIAN_POINT('',(2.89176323702264,1.72,4.05251606177196));
#5222=CARTESIAN_POINT('',(2.89176323702264,1.72,4.05251606177196));
#5223=CARTESIAN_POINT('Origin',(2.44948723543241,1.72,4.42362961818127));
#5224=CARTESIAN_POINT('',(2.44948723543241,1.72,4.42362961818127));
#5225=CARTESIAN_POINT('',(2.44948723543241,1.72,4.42362961818127));
#5226=CARTESIAN_POINT('',(2.44948723543241,1.72,4.42362961818127));
#5227=CARTESIAN_POINT('Origin',(1.90695546709804,1.72,4.22616414352457));
#5228=CARTESIAN_POINT('',(1.90695546709804,1.72,4.22616414352457));
#5229=CARTESIAN_POINT('',(1.90695546709804,1.72,4.22616414352457));
#5230=CARTESIAN_POINT('',(1.90695546709804,1.72,4.22616414352457));
#5231=CARTESIAN_POINT('Origin',(1.80669970035391,1.72,3.65758511245857));
#5232=CARTESIAN_POINT('',(1.80669970035391,1.72,3.65758511245857));
#5233=CARTESIAN_POINT('',(1.80669970035391,1.72,3.65758511245857));
#5234=CARTESIAN_POINT('',(1.80669970035391,1.72,3.65758511245857));
#5235=CARTESIAN_POINT('Origin',(2.24897570194414,1.72,3.28647155604926));
#5236=CARTESIAN_POINT('',(2.24897570194414,1.72,3.28647155604926));
#5237=CARTESIAN_POINT('Origin',(2.34923146868827,2.12000000000004,3.85505058711526));
#5238=CARTESIAN_POINT('Origin',(2.34923146868827,1.72,3.85505058711526));
#5239=CARTESIAN_POINT('',(0.,0.,0.));
#5240=CARTESIAN_POINT('Origin',(2.34923146868827,1.56,3.85505058711526));
#5241=CARTESIAN_POINT('',(2.04852984069618,1.72000000000002,3.74560411196451));
#5242=CARTESIAN_POINT('Origin',(2.34923146868827,1.72000000000002,3.85505058711526));
#5243=CARTESIAN_POINT('',(2.04852984069618,1.56,3.74560411196451));
#5244=CARTESIAN_POINT('',(2.04852984069618,1.56,3.74560411196451));
#5245=CARTESIAN_POINT('Origin',(2.34923146868827,1.56,3.85505058711526));
#5246=CARTESIAN_POINT('Origin',(2.34923146868827,1.56,3.85505058711526));
#5247=CARTESIAN_POINT('',(1.78541591620309,1.72000000000002,3.6498384462076));
#5248=CARTESIAN_POINT('Origin',(2.34923146868827,1.72000000000002,3.85505058711526));
#5249=CARTESIAN_POINT('',(1.78541591620309,1.56,3.6498384462076));
#5250=CARTESIAN_POINT('',(1.78541591620309,1.56,3.6498384462076));
#5251=CARTESIAN_POINT('Origin',(2.34923146868827,1.56,3.85505058711526));
#5252=CARTESIAN_POINT('Origin',(2.34923146868827,1.72000000000002,3.85505058711526));
#5253=CARTESIAN_POINT('Origin',(2.34923146868827,1.56,3.85505058711526));
#5254=CARTESIAN_POINT('',(0.,0.,0.));
#5255=CARTESIAN_POINT('Origin',(2.34923146868827,-1.72,3.85505058711526));
#5256=CARTESIAN_POINT('',(2.04852984069618,-1.55999999999998,3.74560411196451));
#5257=CARTESIAN_POINT('Origin',(2.34923146868827,-1.55999999999998,3.85505058711526));
#5258=CARTESIAN_POINT('',(2.04852984069618,-1.72,3.74560411196451));
#5259=CARTESIAN_POINT('',(2.04852984069618,-1.72,3.74560411196451));
#5260=CARTESIAN_POINT('Origin',(2.34923146868827,-1.72,3.85505058711526));
#5261=CARTESIAN_POINT('Origin',(2.34923146868827,-1.72,3.85505058711526));
#5262=CARTESIAN_POINT('',(1.78541591620309,-1.55999999999998,3.6498384462076));
#5263=CARTESIAN_POINT('Origin',(2.34923146868827,-1.55999999999998,3.85505058711526));
#5264=CARTESIAN_POINT('',(1.78541591620309,-1.72,3.6498384462076));
#5265=CARTESIAN_POINT('',(1.78541591620309,-1.72,3.6498384462076));
#5266=CARTESIAN_POINT('Origin',(2.34923146868827,-1.72,3.85505058711526));
#5267=CARTESIAN_POINT('Origin',(2.34923146868827,-1.55999999999998,3.85505058711526));
#5268=CARTESIAN_POINT('Origin',(2.34923146868827,-1.72,3.85505058711526));
#5269=CARTESIAN_POINT('',(0.,0.,0.));
#5270=CARTESIAN_POINT('Origin',(2.34923146868827,-2.18158650880638,3.85505058711526));
#5271=CARTESIAN_POINT('',(1.90695546709804,-2.18090804453173,4.22616414352457));
#5272=CARTESIAN_POINT('',(2.44948723543241,-2.18090804453173,4.42362961818127));
#5273=CARTESIAN_POINT('Ctrl Pts',(1.90695546709804,-2.18090804453173,4.22616414352457));
#5274=CARTESIAN_POINT('Ctrl Pts',(2.17822135126726,-2.2642413778637,4.32489688085366));
#5275=CARTESIAN_POINT('Ctrl Pts',(2.44948723543241,-2.18090804453173,4.42362961818127));
#5276=CARTESIAN_POINT('',(1.80669970035391,-2.18090804453173,3.65758511245857));
#5277=CARTESIAN_POINT('Ctrl Pts',(1.80669970035391,-2.18090804453173,3.65758511245857));
#5278=CARTESIAN_POINT('Ctrl Pts',(1.85682758372635,-2.2642413778637,3.9418746279937));
#5279=CARTESIAN_POINT('Ctrl Pts',(1.90695546709804,-2.18090804453173,4.22616414352457));
#5280=CARTESIAN_POINT('',(1.9028774896375,-2.24,3.69259097556336));
#5281=CARTESIAN_POINT('',(1.80780396562194,-2.18158650880638,3.65798703226866));
#5282=CARTESIAN_POINT('Origin',(2.34923146868827,-2.24,3.85505058711526));
#5283=CARTESIAN_POINT('',(2.24897570194414,-2.18090804453173,3.28647155604926));
#5284=CARTESIAN_POINT('Ctrl Pts',(2.24897570194414,-2.18090804453173,3.28647155604926));
#5285=CARTESIAN_POINT('Ctrl Pts',(2.02783770114737,-2.2642413778637,3.47202833425531));
#5286=CARTESIAN_POINT('Ctrl Pts',(1.80669970035391,-2.18090804453173,3.65758511245857));
#5287=CARTESIAN_POINT('',(2.79150747027851,-2.18090804453173,3.48393703070596));
#5288=CARTESIAN_POINT('Ctrl Pts',(2.79150747027851,-2.18090804453173,3.48393703070596));
#5289=CARTESIAN_POINT('Ctrl Pts',(2.52024158610929,-2.2642413778637,3.38520429337687));
#5290=CARTESIAN_POINT('Ctrl Pts',(2.24897570194414,-2.18090804453173,3.28647155604926));
#5291=CARTESIAN_POINT('',(2.89176323702264,-2.18090804453173,4.05251606177196));
#5292=CARTESIAN_POINT('Ctrl Pts',(2.89176323702264,-2.18090804453173,4.05251606177196));
#5293=CARTESIAN_POINT('Ctrl Pts',(2.8416353536502,-2.2642413778637,3.76822654623683));
#5294=CARTESIAN_POINT('Ctrl Pts',(2.79150747027851,-2.18090804453173,3.48393703070596));
#5295=CARTESIAN_POINT('Ctrl Pts',(2.44948723543241,-2.18090804453173,4.42362961818127));
#5296=CARTESIAN_POINT('Ctrl Pts',(2.67062523622918,-2.2642413778637,4.23807283997522));
#5297=CARTESIAN_POINT('Ctrl Pts',(2.89176323702264,-2.18090804453173,4.05251606177196));
#5298=CARTESIAN_POINT('Origin',(2.34923146868827,-1.77841349119356,3.85505058711526));
#5299=CARTESIAN_POINT('',(1.9028774896375,-1.71999999999994,3.69259097556336));
#5300=CARTESIAN_POINT('Origin',(2.34923146868827,-1.71999999999994,3.85505058711526));
#5301=CARTESIAN_POINT('',(1.80669970035391,-1.77909195546821,3.65758511245857));
#5302=CARTESIAN_POINT('',(1.80780396562194,-1.77841349119356,3.65798703226866));
#5303=CARTESIAN_POINT('',(1.90695546709804,-1.77909195546821,4.22616414352457));
#5304=CARTESIAN_POINT('Ctrl Pts',(1.90695546709804,-1.77909195546821,4.22616414352457));
#5305=CARTESIAN_POINT('Ctrl Pts',(1.8568275837256,-1.69575862213624,3.94187462798943));
#5306=CARTESIAN_POINT('Ctrl Pts',(1.80669970035391,-1.77909195546821,3.65758511245857));
#5307=CARTESIAN_POINT('',(2.44948723543241,-1.77909195546821,4.42362961818127));
#5308=CARTESIAN_POINT('Ctrl Pts',(2.44948723543241,-1.77909195546821,4.42362961818127));
#5309=CARTESIAN_POINT('Ctrl Pts',(2.17822135126319,-1.69575862213624,4.32489688085218));
#5310=CARTESIAN_POINT('Ctrl Pts',(1.90695546709804,-1.77909195546821,4.22616414352457));
#5311=CARTESIAN_POINT('',(2.89176323702264,-1.77909195546821,4.05251606177196));
#5312=CARTESIAN_POINT('Ctrl Pts',(2.89176323702264,-1.77909195546821,4.05251606177196));
#5313=CARTESIAN_POINT('Ctrl Pts',(2.67062523622586,-1.69575862213624,4.23807283997801));
#5314=CARTESIAN_POINT('Ctrl Pts',(2.44948723543241,-1.77909195546821,4.42362961818127));
#5315=CARTESIAN_POINT('',(2.79150747027851,-1.77909195546821,3.48393703070596));
#5316=CARTESIAN_POINT('Ctrl Pts',(2.79150747027851,-1.77909195546821,3.48393703070596));
#5317=CARTESIAN_POINT('Ctrl Pts',(2.84163535365095,-1.69575862213624,3.76822654624109));
#5318=CARTESIAN_POINT('Ctrl Pts',(2.89176323702264,-1.77909195546821,4.05251606177196));
#5319=CARTESIAN_POINT('',(2.24897570194414,-1.77909195546821,3.28647155604926));
#5320=CARTESIAN_POINT('Ctrl Pts',(2.24897570194414,-1.77909195546821,3.28647155604926));
#5321=CARTESIAN_POINT('Ctrl Pts',(2.52024158611336,-1.69575862213624,3.38520429337835));
#5322=CARTESIAN_POINT('Ctrl Pts',(2.79150747027851,-1.77909195546821,3.48393703070596));
#5323=CARTESIAN_POINT('Ctrl Pts',(1.80669970035391,-1.77909195546821,3.65758511245857));
#5324=CARTESIAN_POINT('Ctrl Pts',(2.02783770115069,-1.69575862213624,3.47202833425252));
#5325=CARTESIAN_POINT('Ctrl Pts',(2.24897570194414,-1.77909195546821,3.28647155604926));
#5326=CARTESIAN_POINT('Origin',(2.79150747027851,-2.24,3.48393703070596));
#5327=CARTESIAN_POINT('',(2.24897570194414,-2.24,3.28647155604926));
#5328=CARTESIAN_POINT('',(2.79150747027851,-2.24,3.48393703070596));
#5329=CARTESIAN_POINT('Origin',(2.24897570194414,-2.24,3.28647155604926));
#5330=CARTESIAN_POINT('',(1.80669970035391,-2.24,3.65758511245857));
#5331=CARTESIAN_POINT('Origin',(1.80669970035391,-2.24,3.65758511245857));
#5332=CARTESIAN_POINT('',(1.90695546709804,-2.24,4.22616414352457));
#5333=CARTESIAN_POINT('Origin',(2.34923146868827,-2.24,3.85505058711526));
#5334=CARTESIAN_POINT('',(2.11266385979137,-1.71999999999994,3.76894699299276));
#5335=CARTESIAN_POINT('Origin',(2.34923146868827,-1.71999999999994,3.85505058711526));
#5336=CARTESIAN_POINT('',(2.11266385979137,-2.24,3.76894699299276));
#5337=CARTESIAN_POINT('',(2.11266385979137,-2.24,3.76894699299276));
#5338=CARTESIAN_POINT('Origin',(2.34923146868827,-2.24,3.85505058711526));
#5339=CARTESIAN_POINT('Origin',(1.90695546709804,-2.24,4.22616414352457));
#5340=CARTESIAN_POINT('',(2.44948723543241,-2.24,4.42362961818127));
#5341=CARTESIAN_POINT('Origin',(2.89176323702264,-2.24,4.05251606177196));
#5342=CARTESIAN_POINT('',(2.89176323702264,-2.24,4.05251606177196));
#5343=CARTESIAN_POINT('Origin',(2.44948723543241,-2.24,4.42362961818127));
#5344=CARTESIAN_POINT('Origin',(2.34923146868827,-1.71999999999994,3.85505058711526));
#5345=CARTESIAN_POINT('Origin',(2.34923146868827,-2.24,3.85505058711526));
#5346=CARTESIAN_POINT('',(0.,0.,0.));
#5347=CARTESIAN_POINT('',(0.,0.,0.));
#5348=CARTESIAN_POINT('',(0.,0.,0.));
#5349=CARTESIAN_POINT('',(0.,0.,0.));
#5350=CARTESIAN_POINT('',(0.,0.,0.));
#5351=CARTESIAN_POINT('',(0.,0.,0.));
#5352=CARTESIAN_POINT('',(0.,0.,0.));
#5353=CARTESIAN_POINT('',(0.,0.,0.));
#5354=CARTESIAN_POINT('',(0.,0.,0.));
#5355=CARTESIAN_POINT('',(0.,0.,0.));
#5356=CARTESIAN_POINT('',(0.,0.,0.));
#5357=CARTESIAN_POINT('',(0.,0.,0.));
#5358=CARTESIAN_POINT('',(0.,0.,0.));
#5359=CARTESIAN_POINT('Origin',(21.5,-1.2,-0.1));
#5360=CARTESIAN_POINT('',(21.225,-1.2,0.));
#5361=CARTESIAN_POINT('Origin',(21.5,-1.2,0.));
#5362=CARTESIAN_POINT('',(21.225,-1.2,0.5));
#5363=CARTESIAN_POINT('',(21.225,-1.2,-0.1));
#5364=CARTESIAN_POINT('Origin',(21.5,-1.2,0.5));
#5365=CARTESIAN_POINT('Origin',(21.5,1.2,-0.1));
#5366=CARTESIAN_POINT('',(21.225,1.2,0.));
#5367=CARTESIAN_POINT('Origin',(21.5,1.2,0.));
#5368=CARTESIAN_POINT('',(21.225,1.2,0.5));
#5369=CARTESIAN_POINT('',(21.225,1.2,-0.1));
#5370=CARTESIAN_POINT('Origin',(21.5,1.2,0.5));
#5371=CARTESIAN_POINT('Origin',(20.,-1.7,3.));
#5372=CARTESIAN_POINT('',(19.59,-1.55,3.));
#5373=CARTESIAN_POINT('Origin',(20.,-1.55,3.));
#5374=CARTESIAN_POINT('',(19.59,-1.25,3.));
#5375=CARTESIAN_POINT('',(19.59,-1.7,3.));
#5376=CARTESIAN_POINT('Origin',(20.,-1.25,3.));
#5377=CARTESIAN_POINT('Origin',(20.,-1.7,3.));
#5378=CARTESIAN_POINT('',(19.59,1.25,3.));
#5379=CARTESIAN_POINT('Origin',(20.,1.25,3.));
#5380=CARTESIAN_POINT('',(19.59,1.55,3.));
#5381=CARTESIAN_POINT('',(19.59,-1.7,3.));
#5382=CARTESIAN_POINT('Origin',(20.,1.55,3.));
#5383=CARTESIAN_POINT('Origin',(20.,1.25,3.));
#5384=CARTESIAN_POINT('',(19.6,1.25,2.4255437353462));
#5385=CARTESIAN_POINT('',(19.6,1.55,2.4255437353462));
#5386=CARTESIAN_POINT('',(19.6,1.25,2.4255437353462));
#5387=CARTESIAN_POINT('',(20.4,1.25,2.4255437353462));
#5388=CARTESIAN_POINT('Origin',(20.,1.25,3.));
#5389=CARTESIAN_POINT('',(20.4,1.55,2.4255437353462));
#5390=CARTESIAN_POINT('',(20.4,1.25,2.4255437353462));
#5391=CARTESIAN_POINT('Origin',(20.,1.55,3.));
#5392=CARTESIAN_POINT('Origin',(20.,1.55,1.7));
#5393=CARTESIAN_POINT('',(20.4,1.55,0.5));
#5394=CARTESIAN_POINT('',(20.4,1.55,0.4));
#5395=CARTESIAN_POINT('',(20.,1.55,0.5));
#5396=CARTESIAN_POINT('',(20.75,1.55,0.5));
#5397=CARTESIAN_POINT('',(20.,1.55,0.4));
#5398=CARTESIAN_POINT('',(20.,1.55,0.85));
#5399=CARTESIAN_POINT('',(19.6,1.55,0.4));
#5400=CARTESIAN_POINT('',(19.6,1.55,0.4));
#5401=CARTESIAN_POINT('',(19.6,1.55,3.));
#5402=CARTESIAN_POINT('Origin',(20.4,1.25,3.));
#5403=CARTESIAN_POINT('',(20.4,1.25,0.5));
#5404=CARTESIAN_POINT('',(20.4,1.25,0.4));
#5405=CARTESIAN_POINT('',(20.4,0.625,0.5));
#5406=CARTESIAN_POINT('Origin',(20.,1.25,1.7));
#5407=CARTESIAN_POINT('',(19.6,1.25,0.4));
#5408=CARTESIAN_POINT('',(19.6,1.25,3.));
#5409=CARTESIAN_POINT('',(20.,1.25,0.4));
#5410=CARTESIAN_POINT('',(19.6,1.25,0.4));
#5411=CARTESIAN_POINT('',(20.,1.25,0.5));
#5412=CARTESIAN_POINT('',(20.,1.25,0.85));
#5413=CARTESIAN_POINT('',(20.75,1.25,0.5));
#5414=CARTESIAN_POINT('Origin',(19.6,1.25,0.4));
#5415=CARTESIAN_POINT('',(19.6,1.25,0.4));
#5416=CARTESIAN_POINT('Origin',(20.4,1.25,0.4));
#5417=CARTESIAN_POINT('',(20.,1.625,0.4));
#5418=CARTESIAN_POINT('Origin',(20.,2.,0.));
#5419=CARTESIAN_POINT('',(20.,2.,0.5));
#5420=CARTESIAN_POINT('',(20.,2.,0.5));
#5421=CARTESIAN_POINT('',(20.,2.,0.));
#5422=CARTESIAN_POINT('',(20.,2.,0.));
#5423=CARTESIAN_POINT('',(20.,-2.,0.));
#5424=CARTESIAN_POINT('',(20.,2.,0.));
#5425=CARTESIAN_POINT('',(20.,-2.,0.5));
#5426=CARTESIAN_POINT('',(20.,-2.,0.));
#5427=CARTESIAN_POINT('',(20.,-1.55,0.5));
#5428=CARTESIAN_POINT('',(20.,2.,0.5));
#5429=CARTESIAN_POINT('',(20.,-1.55,0.4));
#5430=CARTESIAN_POINT('',(20.,-1.55,0.85));
#5431=CARTESIAN_POINT('',(20.,-1.25,0.4));
#5432=CARTESIAN_POINT('',(20.,0.225,0.4));
#5433=CARTESIAN_POINT('',(20.,-1.25,0.5));
#5434=CARTESIAN_POINT('',(20.,-1.25,0.85));
#5435=CARTESIAN_POINT('',(20.,2.,0.5));
#5436=CARTESIAN_POINT('Origin',(20.,-1.55,3.));
#5437=CARTESIAN_POINT('',(19.6,-1.55,2.4255437353462));
#5438=CARTESIAN_POINT('',(19.6,-1.25,2.4255437353462));
#5439=CARTESIAN_POINT('',(19.6,-1.55,2.4255437353462));
#5440=CARTESIAN_POINT('',(20.4,-1.55,2.4255437353462));
#5441=CARTESIAN_POINT('Origin',(20.,-1.55,3.));
#5442=CARTESIAN_POINT('',(20.4,-1.25,2.4255437353462));
#5443=CARTESIAN_POINT('',(20.4,-1.55,2.4255437353462));
#5444=CARTESIAN_POINT('Origin',(20.,-1.25,3.));
#5445=CARTESIAN_POINT('Origin',(20.,-1.25,1.7));
#5446=CARTESIAN_POINT('',(20.4,-1.25,0.5));
#5447=CARTESIAN_POINT('',(20.4,-1.25,0.4));
#5448=CARTESIAN_POINT('',(20.75,-1.25,0.5));
#5449=CARTESIAN_POINT('',(19.6,-1.25,0.4));
#5450=CARTESIAN_POINT('',(19.6,-1.25,0.4));
#5451=CARTESIAN_POINT('',(19.6,-1.25,3.));
#5452=CARTESIAN_POINT('Origin',(20.4,-1.55,3.));
#5453=CARTESIAN_POINT('',(20.4,-1.55,0.5));
#5454=CARTESIAN_POINT('',(20.4,-1.55,0.4));
#5455=CARTESIAN_POINT('',(20.4,-0.775,0.5));
#5456=CARTESIAN_POINT('Origin',(20.,-1.55,1.7));
#5457=CARTESIAN_POINT('',(19.6,-1.55,0.4));
#5458=CARTESIAN_POINT('',(19.6,-1.55,3.));
#5459=CARTESIAN_POINT('',(19.6,-1.55,0.4));
#5460=CARTESIAN_POINT('',(20.75,-1.55,0.5));
#5461=CARTESIAN_POINT('Origin',(19.6,-1.55,0.4));
#5462=CARTESIAN_POINT('',(19.6,-1.55,0.4));
#5463=CARTESIAN_POINT('Origin',(20.4,-1.55,0.4));
#5464=CARTESIAN_POINT('Origin',(23.,2.,0.));
#5465=CARTESIAN_POINT('',(23.,2.,0.));
#5466=CARTESIAN_POINT('',(23.,2.,0.));
#5467=CARTESIAN_POINT('',(23.,2.,0.5));
#5468=CARTESIAN_POINT('',(23.,2.,0.5));
#5469=CARTESIAN_POINT('',(23.,2.,0.));
#5470=CARTESIAN_POINT('Origin',(23.,-2.,0.));
#5471=CARTESIAN_POINT('',(23.,-2.,0.));
#5472=CARTESIAN_POINT('',(23.,-2.,0.));
#5473=CARTESIAN_POINT('',(23.,-2.,0.5));
#5474=CARTESIAN_POINT('',(23.,-2.,0.5));
#5475=CARTESIAN_POINT('',(23.,-2.,0.));
#5476=CARTESIAN_POINT('Origin',(20.,-2.,0.));
#5477=CARTESIAN_POINT('',(20.,-2.,0.));
#5478=CARTESIAN_POINT('',(20.,-2.,0.5));
#5479=CARTESIAN_POINT('Origin',(21.5,0.,0.5));
#5480=CARTESIAN_POINT('Origin',(21.5,0.,0.));
#5481=CARTESIAN_POINT('',(0.,0.,0.));
#5482=CARTESIAN_POINT('',(0.,0.,0.));
#5483=CARTESIAN_POINT('',(0.,0.,0.));
#5484=CARTESIAN_POINT('Origin',(0.,-1.7,3.));
#5485=CARTESIAN_POINT('',(-0.41,-1.52,3.));
#5486=CARTESIAN_POINT('Origin',(0.,-1.52,3.));
#5487=CARTESIAN_POINT('',(-0.41,-1.28,3.));
#5488=CARTESIAN_POINT('',(-0.41,-1.7,3.));
#5489=CARTESIAN_POINT('',(2.22044604925031E-16,-1.28,3.41));
#5490=CARTESIAN_POINT('Origin',(0.,-1.28,3.));
#5491=CARTESIAN_POINT('',(2.22044604925031E-16,-1.28,2.59));
#5492=CARTESIAN_POINT('Origin',(0.,-1.28,3.));
#5493=CARTESIAN_POINT('Origin',(0.,-1.28,3.));
#5494=CARTESIAN_POINT('Origin',(0.,-1.7,3.));
#5495=CARTESIAN_POINT('',(-1.73201719910321E-17,1.28,3.41));
#5496=CARTESIAN_POINT('',(-1.73201719910321E-17,1.28,2.59));
#5497=CARTESIAN_POINT('Origin',(0.,1.28,3.));
#5498=CARTESIAN_POINT('',(-0.41,1.28,3.));
#5499=CARTESIAN_POINT('Origin',(0.,1.28,3.));
#5500=CARTESIAN_POINT('',(-0.41,1.52,3.));
#5501=CARTESIAN_POINT('',(-0.41,-1.7,3.));
#5502=CARTESIAN_POINT('Origin',(0.,1.52,3.));
#5503=CARTESIAN_POINT('Origin',(0.,1.28,3.));
#5504=CARTESIAN_POINT('Origin',(2.5,-1.7,3.));
#5505=CARTESIAN_POINT('',(2.5,-1.12,3.41));
#5506=CARTESIAN_POINT('',(2.5,-1.12,2.59));
#5507=CARTESIAN_POINT('Origin',(2.5,-1.12,3.));
#5508=CARTESIAN_POINT('',(2.09,-1.1856,3.));
#5509=CARTESIAN_POINT('Origin',(2.5,-1.12,3.));
#5510=CARTESIAN_POINT('',(2.09,-0.88,3.));
#5511=CARTESIAN_POINT('',(2.09,-1.7,3.));
#5512=CARTESIAN_POINT('Origin',(2.5,-0.88,3.));
#5513=CARTESIAN_POINT('Origin',(2.5,-1.12,3.));
#5514=CARTESIAN_POINT('Origin',(2.5,-1.7,3.));
#5515=CARTESIAN_POINT('',(2.09,0.88,3.));
#5516=CARTESIAN_POINT('Origin',(2.5,0.88,3.));
#5517=CARTESIAN_POINT('',(2.09,1.1856,3.));
#5518=CARTESIAN_POINT('',(2.09,-1.7,3.));
#5519=CARTESIAN_POINT('',(2.5,1.12,3.41));
#5520=CARTESIAN_POINT('Origin',(2.5,1.12,3.));
#5521=CARTESIAN_POINT('',(2.5,1.12,2.59));
#5522=CARTESIAN_POINT('Origin',(2.5,1.12,3.));
#5523=CARTESIAN_POINT('Origin',(2.5,1.12,3.));
#5524=CARTESIAN_POINT('Origin',(0.,1.28,3.));
#5525=CARTESIAN_POINT('',(0.,1.28,3.7));
#5526=CARTESIAN_POINT('',(-1.73201719910321E-17,1.28,2.));
#5527=CARTESIAN_POINT('',(0.,1.28,2.3));
#5528=CARTESIAN_POINT('Origin',(0.,1.28,3.));
#5529=CARTESIAN_POINT('',(-1.73201719910321E-17,1.28,2.));
#5530=CARTESIAN_POINT('Origin',(0.,-1.28,3.));
#5531=CARTESIAN_POINT('',(0.,-1.28,2.3));
#5532=CARTESIAN_POINT('',(2.22044604925031E-16,-1.28,2.));
#5533=CARTESIAN_POINT('',(0.,-1.28,3.7));
#5534=CARTESIAN_POINT('Origin',(0.,-1.28,3.));
#5535=CARTESIAN_POINT('',(2.22044604925031E-16,-1.28,2.));
#5536=CARTESIAN_POINT('Origin',(2.5,1.12,1.));
#5537=CARTESIAN_POINT('',(2.5,1.12,2.3));
#5538=CARTESIAN_POINT('',(2.5,1.12,1.));
#5539=CARTESIAN_POINT('',(2.5,1.12,1.));
#5540=CARTESIAN_POINT('',(2.5,1.12,1.));
#5541=CARTESIAN_POINT('',(0.,1.52,1.));
#5542=CARTESIAN_POINT('',(2.5,1.12,1.));
#5543=CARTESIAN_POINT('',(0.,1.52,2.3));
#5544=CARTESIAN_POINT('',(0.,1.52,1.));
#5545=CARTESIAN_POINT('',(0.,1.52,3.7));
#5546=CARTESIAN_POINT('Origin',(0.,1.52,3.));
#5547=CARTESIAN_POINT('',(2.5,1.12,3.7));
#5548=CARTESIAN_POINT('',(2.5,1.12,3.7));
#5549=CARTESIAN_POINT('',(2.5,1.12,1.));
#5550=CARTESIAN_POINT('Origin',(0.,-1.52,1.));
#5551=CARTESIAN_POINT('',(2.5,-1.12,3.7));
#5552=CARTESIAN_POINT('',(2.5,-1.12,1.));
#5553=CARTESIAN_POINT('',(0.,-1.52,3.7));
#5554=CARTESIAN_POINT('',(0.,-1.52,3.7));
#5555=CARTESIAN_POINT('',(0.,-1.52,2.3));
#5556=CARTESIAN_POINT('Origin',(0.,-1.52,3.));
#5557=CARTESIAN_POINT('',(0.,-1.52,1.));
#5558=CARTESIAN_POINT('',(0.,-1.52,1.));
#5559=CARTESIAN_POINT('',(2.5,-1.12,1.));
#5560=CARTESIAN_POINT('',(0.,-1.52,1.));
#5561=CARTESIAN_POINT('',(2.5,-1.12,2.3));
#5562=CARTESIAN_POINT('',(2.5,-1.12,1.));
#5563=CARTESIAN_POINT('',(2.5,-1.12,1.));
#5564=CARTESIAN_POINT('Origin',(0.8,1.3,1.));
#5565=CARTESIAN_POINT('',(0.8,-1.152,1.3));
#5566=CARTESIAN_POINT('',(0.8,-1.152,1.));
#5567=CARTESIAN_POINT('',(0.8,-1.152,1.));
#5568=CARTESIAN_POINT('',(0.8,1.152,1.3));
#5569=CARTESIAN_POINT('',(0.8,1.3,1.3));
#5570=CARTESIAN_POINT('',(0.8,1.152,1.));
#5571=CARTESIAN_POINT('',(0.8,1.152,1.));
#5572=CARTESIAN_POINT('',(0.8,1.3,1.));
#5573=CARTESIAN_POINT('Origin',(1.7,-1.15,1.));
#5574=CARTESIAN_POINT('',(1.7,-1.008,1.));
#5575=CARTESIAN_POINT('',(1.7,-1.008,1.3));
#5576=CARTESIAN_POINT('',(1.7,-1.008,1.));
#5577=CARTESIAN_POINT('',(1.7,1.008,1.));
#5578=CARTESIAN_POINT('',(1.7,-1.15,1.));
#5579=CARTESIAN_POINT('',(1.7,1.008,1.3));
#5580=CARTESIAN_POINT('',(1.7,1.008,1.));
#5581=CARTESIAN_POINT('',(1.7,-1.15,1.3));
#5582=CARTESIAN_POINT('Origin',(1.25,0.,1.3));
#5583=CARTESIAN_POINT('',(1.95924336973479,-0.966521060842434,1.3));
#5584=CARTESIAN_POINT('',(0.709243369734789,1.16652106084243,1.3));
#5585=CARTESIAN_POINT('Origin',(2.5,0.88,3.));
#5586=CARTESIAN_POINT('',(2.5,0.88,2.3));
#5587=CARTESIAN_POINT('',(2.5,0.88,3.7));
#5588=CARTESIAN_POINT('Origin',(2.5,0.88,3.));
#5589=CARTESIAN_POINT('Origin',(2.5,0.88,3.));
#5590=CARTESIAN_POINT('Origin',(2.5,0.88,3.));
#5591=CARTESIAN_POINT('',(2.5,0.88,2.3));
#5592=CARTESIAN_POINT('Origin',(2.5,1.12,3.));
#5593=CARTESIAN_POINT('',(2.5,0.88,3.7));
#5594=CARTESIAN_POINT('Origin',(2.5,1.12,3.));
#5595=CARTESIAN_POINT('Origin',(2.5,0.88,3.));
#5596=CARTESIAN_POINT('Origin',(2.5,0.88,3.));
#5597=CARTESIAN_POINT('Origin',(0.,1.28,1.));
#5598=CARTESIAN_POINT('',(0.,1.28,1.));
#5599=CARTESIAN_POINT('',(0.,1.28,1.));
#5600=CARTESIAN_POINT('',(0.,1.28,1.));
#5601=CARTESIAN_POINT('',(2.5,0.88,1.));
#5602=CARTESIAN_POINT('',(0.,1.28,1.));
#5603=CARTESIAN_POINT('',(2.5,0.88,1.));
#5604=CARTESIAN_POINT('',(0.,1.28,3.7));
#5605=CARTESIAN_POINT('Origin',(2.5,0.88,1.));
#5606=CARTESIAN_POINT('',(2.5,0.88,1.));
#5607=CARTESIAN_POINT('Origin',(0.,1.52,1.));
#5608=CARTESIAN_POINT('',(0.,1.28,2.3));
#5609=CARTESIAN_POINT('',(0.,1.52,1.));
#5610=CARTESIAN_POINT('Origin',(1.25,1.2,3.7));
#5611=CARTESIAN_POINT('',(0.,1.28,3.7));
#5612=CARTESIAN_POINT('Origin',(0.,1.28,3.));
#5613=CARTESIAN_POINT('Origin',(0.,1.52,3.));
#5614=CARTESIAN_POINT('Origin',(0.,1.28,3.));
#5615=CARTESIAN_POINT('Origin',(0.,1.52,3.));
#5616=CARTESIAN_POINT('Origin',(0.,1.52,3.));
#5617=CARTESIAN_POINT('Origin',(2.5,-0.88,1.));
#5618=CARTESIAN_POINT('',(2.5,-0.88,3.7));
#5619=CARTESIAN_POINT('',(2.5,-0.88,3.7));
#5620=CARTESIAN_POINT('',(2.5,-0.88,2.3));
#5621=CARTESIAN_POINT('Origin',(2.5,-0.88,3.));
#5622=CARTESIAN_POINT('',(2.5,-0.88,1.));
#5623=CARTESIAN_POINT('',(2.5,-0.88,1.));
#5624=CARTESIAN_POINT('',(2.5,-0.88,1.));
#5625=CARTESIAN_POINT('',(0.,-1.28,1.));
#5626=CARTESIAN_POINT('',(2.5,-0.88,1.));
#5627=CARTESIAN_POINT('',(0.,-1.28,1.));
#5628=CARTESIAN_POINT('Origin',(2.5,-0.88,3.));
#5629=CARTESIAN_POINT('Origin',(2.5,-0.88,3.));
#5630=CARTESIAN_POINT('Origin',(2.5,-0.88,3.));
#5631=CARTESIAN_POINT('Origin',(2.5,-1.12,3.));
#5632=CARTESIAN_POINT('Origin',(2.5,-1.12,3.));
#5633=CARTESIAN_POINT('',(2.5,-1.12,2.3));
#5634=CARTESIAN_POINT('',(2.5,-1.12,3.7));
#5635=CARTESIAN_POINT('Origin',(2.5,-1.12,3.));
#5636=CARTESIAN_POINT('Origin',(2.5,-1.12,3.));
#5637=CARTESIAN_POINT('Origin',(2.5,-1.12,1.));
#5638=CARTESIAN_POINT('',(2.5,-1.12,1.));
#5639=CARTESIAN_POINT('Origin',(0.,-1.28,1.));
#5640=CARTESIAN_POINT('',(0.,-1.52,2.3));
#5641=CARTESIAN_POINT('',(0.,-1.28,1.));
#5642=CARTESIAN_POINT('Origin',(1.25,-1.2,3.7));
#5643=CARTESIAN_POINT('',(0.,-1.52,3.7));
#5644=CARTESIAN_POINT('Origin',(1.25,-1.2,1.));
#5645=CARTESIAN_POINT('Origin',(0.,-1.52,3.));
#5646=CARTESIAN_POINT('Origin',(0.,-1.52,3.));
#5647=CARTESIAN_POINT('Origin',(0.,-1.52,3.));
#5648=CARTESIAN_POINT('Origin',(0.,-1.52,3.));
#5649=CARTESIAN_POINT('Origin',(0.,-1.52,3.));
#5650=CARTESIAN_POINT('',(0.,0.,0.));
#5651=CARTESIAN_POINT('Origin',(0.,-1.56,3.));
#5652=CARTESIAN_POINT('',(-0.31,1.56,3.));
#5653=CARTESIAN_POINT('Origin',(0.,1.56,3.));
#5654=CARTESIAN_POINT('',(-0.31,-1.56,3.));
#5655=CARTESIAN_POINT('',(-0.31,-1.56,3.));
#5656=CARTESIAN_POINT('Origin',(0.,-1.56,3.));
#5657=CARTESIAN_POINT('Origin',(0.,-1.56,3.));
#5658=CARTESIAN_POINT('',(-0.4,1.56,3.));
#5659=CARTESIAN_POINT('Origin',(0.,1.56,3.));
#5660=CARTESIAN_POINT('',(-0.4,-1.56,3.));
#5661=CARTESIAN_POINT('',(-0.4,-1.56,3.));
#5662=CARTESIAN_POINT('Origin',(0.,-1.56,3.));
#5663=CARTESIAN_POINT('Origin',(0.,1.56,3.));
#5664=CARTESIAN_POINT('Origin',(0.,-1.56,3.));
#5665=CARTESIAN_POINT('',(0.,0.,0.));
#5666=CARTESIAN_POINT('Origin',(0.,-2.99,0.));
#5667=CARTESIAN_POINT('',(-0.3,-2.99,3.67394039744206E-17));
#5668=CARTESIAN_POINT('Origin',(0.,-2.99,0.));
#5669=CARTESIAN_POINT('',(-0.25,-2.99,3.06161699786838E-17));
#5670=CARTESIAN_POINT('Origin',(0.,-2.99,0.));
#5671=CARTESIAN_POINT('Origin',(0.,-4.,0.));
#5672=CARTESIAN_POINT('',(-0.3,-4.,3.67394039744206E-17));
#5673=CARTESIAN_POINT('',(-0.3,-4.,3.67394039744206E-17));
#5674=CARTESIAN_POINT('Origin',(0.,-4.,0.));
#5675=CARTESIAN_POINT('Origin',(0.,-4.,0.));
#5676=CARTESIAN_POINT('Origin',(0.,-1.445,0.));
#5677=CARTESIAN_POINT('',(-0.2942,-2.9458,3.60291088309151E-17));
#5678=CARTESIAN_POINT('Origin',(0.,-2.9458,0.));
#5679=CARTESIAN_POINT('',(-0.2942,0.,-3.60291088309151E-17));
#5680=CARTESIAN_POINT('',(-0.2942,-1.445,-3.60291088309151E-17));
#5681=CARTESIAN_POINT('Origin',(0.,0.,0.));
#5682=CARTESIAN_POINT('Origin',(0.,-2.97,0.));
#5683=CARTESIAN_POINT('',(-0.27,-2.97,-3.30654635769785E-17));
#5684=CARTESIAN_POINT('Origin',(0.,0.341586508806388,0.));
#5685=CARTESIAN_POINT('',(-0.475,0.4,-5.81707229594993E-17));
#5686=CARTESIAN_POINT('Origin',(0.,0.4,0.));
#5687=CARTESIAN_POINT('',(-0.577350269189626,0.340908044531739,-7.07050159149938E-17));
#5688=CARTESIAN_POINT('',(-0.576175134594813,0.341586508806388,-7.05611034329833E-17));
#5689=CARTESIAN_POINT('',(-0.288675134594813,0.340908044531739,0.5));
#5690=CARTESIAN_POINT('Ctrl Pts',(-0.288675134594813,0.340908044531739,
0.5));
#5691=CARTESIAN_POINT('Ctrl Pts',(-0.433012701893303,0.424241377863696,
0.249999999998124));
#5692=CARTESIAN_POINT('Ctrl Pts',(-0.577350269189626,0.340908044531739,
-7.07050159149938E-17));
#5693=CARTESIAN_POINT('',(0.288675134594813,0.340908044531739,0.5));
#5694=CARTESIAN_POINT('Ctrl Pts',(0.288675134594813,0.340908044531739,0.5));
#5695=CARTESIAN_POINT('Ctrl Pts',(-2.16648921025353E-12,0.424241377863696,
0.5));
#5696=CARTESIAN_POINT('Ctrl Pts',(-0.288675134594813,0.340908044531739,
0.5));
#5697=CARTESIAN_POINT('',(0.577350269189626,0.340908044531739,0.));
#5698=CARTESIAN_POINT('Ctrl Pts',(0.577350269189626,0.340908044531739,0.));
#5699=CARTESIAN_POINT('Ctrl Pts',(0.433012701891136,0.424241377863697,0.250000000001876));
#5700=CARTESIAN_POINT('Ctrl Pts',(0.288675134594813,0.340908044531739,0.5));
#5701=CARTESIAN_POINT('',(0.288675134594813,0.340908044531739,-0.5));
#5702=CARTESIAN_POINT('Ctrl Pts',(0.288675134594813,0.340908044531739,-0.5));
#5703=CARTESIAN_POINT('Ctrl Pts',(0.433012701893303,0.424241377863696,-0.249999999998124));
#5704=CARTESIAN_POINT('Ctrl Pts',(0.577350269189626,0.340908044531739,0.));
#5705=CARTESIAN_POINT('',(-0.288675134594813,0.340908044531739,-0.5));
#5706=CARTESIAN_POINT('Ctrl Pts',(-0.288675134594813,0.340908044531739,
-0.5));
#5707=CARTESIAN_POINT('Ctrl Pts',(2.16660023255599E-12,0.424241377863696,
-0.5));
#5708=CARTESIAN_POINT('Ctrl Pts',(0.288675134594813,0.340908044531739,-0.5));
#5709=CARTESIAN_POINT('Ctrl Pts',(-0.577350269189626,0.340908044531739,
-7.07050159149938E-17));
#5710=CARTESIAN_POINT('Ctrl Pts',(-0.433012701891136,0.424241377863697,
-0.250000000001876));
#5711=CARTESIAN_POINT('Ctrl Pts',(-0.288675134594813,0.340908044531739,
-0.5));
#5712=CARTESIAN_POINT('Origin',(0.288675134594813,0.,-0.5));
#5713=CARTESIAN_POINT('',(0.288675134594813,0.,-0.5));
#5714=CARTESIAN_POINT('',(0.288675134594813,0.,-0.5));
#5715=CARTESIAN_POINT('',(-0.288675134594813,0.,-0.5));
#5716=CARTESIAN_POINT('',(0.288675134594813,0.,-0.5));
#5717=CARTESIAN_POINT('',(-0.288675134594813,0.,-0.5));
#5718=CARTESIAN_POINT('Origin',(0.577350269189626,0.,0.));
#5719=CARTESIAN_POINT('',(0.577350269189626,0.,0.));
#5720=CARTESIAN_POINT('',(0.577350269189626,0.,0.));
#5721=CARTESIAN_POINT('',(0.577350269189626,0.,0.));
#5722=CARTESIAN_POINT('Origin',(0.288675134594813,0.,0.5));
#5723=CARTESIAN_POINT('',(0.288675134594813,0.,0.5));
#5724=CARTESIAN_POINT('',(0.288675134594813,0.,0.5));
#5725=CARTESIAN_POINT('',(0.288675134594813,0.,0.5));
#5726=CARTESIAN_POINT('Origin',(-0.288675134594813,0.,0.5));
#5727=CARTESIAN_POINT('',(-0.288675134594813,0.,0.5));
#5728=CARTESIAN_POINT('',(-0.288675134594813,0.,0.5));
#5729=CARTESIAN_POINT('',(-0.288675134594813,0.,0.5));
#5730=CARTESIAN_POINT('Origin',(-0.577350269189626,0.,-7.07050159149938E-17));
#5731=CARTESIAN_POINT('',(-0.577350269189626,0.,-7.07050159149938E-17));
#5732=CARTESIAN_POINT('',(-0.577350269189626,0.,-7.07050159149938E-17));
#5733=CARTESIAN_POINT('',(-0.577350269189626,0.,-7.07050159149938E-17));
#5734=CARTESIAN_POINT('Origin',(-0.288675134594813,0.,-0.5));
#5735=CARTESIAN_POINT('',(-0.288675134594813,0.,-0.5));
#5736=CARTESIAN_POINT('Origin',(0.,0.4,0.));
#5737=CARTESIAN_POINT('Origin',(0.,0.,0.));
#5738=CARTESIAN_POINT('',(0.,0.,0.));
#5739=CARTESIAN_POINT('Origin',(0.,0.,0.));
#5740=CARTESIAN_POINT('',(-0.32,0.16,3.91886975727153E-17));
#5741=CARTESIAN_POINT('Origin',(0.,0.16,0.));
#5742=CARTESIAN_POINT('',(-0.32,0.,3.91886975727153E-17));
#5743=CARTESIAN_POINT('',(-0.32,0.,3.91886975727153E-17));
#5744=CARTESIAN_POINT('Origin',(0.,0.,0.));
#5745=CARTESIAN_POINT('Origin',(0.,0.,0.));
#5746=CARTESIAN_POINT('',(-0.6,0.16,7.34788079488412E-17));
#5747=CARTESIAN_POINT('Origin',(0.,0.16,0.));
#5748=CARTESIAN_POINT('',(-0.6,0.,7.34788079488412E-17));
#5749=CARTESIAN_POINT('',(-0.6,0.,7.34788079488412E-17));
#5750=CARTESIAN_POINT('Origin',(0.,0.,0.));
#5751=CARTESIAN_POINT('Origin',(0.,0.16,0.));
#5752=CARTESIAN_POINT('Origin',(0.,0.,0.));
#5753=CARTESIAN_POINT('',(0.,0.,0.));
#5754=CARTESIAN_POINT('Origin',(0.,0.0584134911936118,0.));
#5755=CARTESIAN_POINT('',(-0.288675134594813,0.0590919554682611,0.5));
#5756=CARTESIAN_POINT('',(0.288675134594813,0.0590919554682611,0.5));
#5757=CARTESIAN_POINT('Ctrl Pts',(-0.288675134594813,0.0590919554682611,
0.5));
#5758=CARTESIAN_POINT('Ctrl Pts',(2.1664336991023E-12,-0.0242413778636964,
0.5));
#5759=CARTESIAN_POINT('Ctrl Pts',(0.288675134594813,0.0590919554682611,
0.5));
#5760=CARTESIAN_POINT('',(-0.577350269189626,0.0590919554682611,-7.07050159149938E-17));
#5761=CARTESIAN_POINT('Ctrl Pts',(-0.577350269189626,0.0590919554682611,
-7.07050159149938E-17));
#5762=CARTESIAN_POINT('Ctrl Pts',(-0.433012701891136,-0.0242413778636963,
0.250000000001876));
#5763=CARTESIAN_POINT('Ctrl Pts',(-0.288675134594813,0.0590919554682611,
0.5));
#5764=CARTESIAN_POINT('',(-0.475,-4.16333634234434E-17,-5.81707229594993E-17));
#5765=CARTESIAN_POINT('',(-0.576175134594813,0.0584134911936118,-7.05611034329833E-17));
#5766=CARTESIAN_POINT('Origin',(0.,0.,0.));
#5767=CARTESIAN_POINT('',(-0.288675134594813,0.0590919554682611,-0.5));
#5768=CARTESIAN_POINT('Ctrl Pts',(-0.288675134594813,0.0590919554682611,
-0.5));
#5769=CARTESIAN_POINT('Ctrl Pts',(-0.433012701893303,-0.0242413778636963,
-0.249999999998124));
#5770=CARTESIAN_POINT('Ctrl Pts',(-0.577350269189626,0.0590919554682611,
-7.07050159149938E-17));
#5771=CARTESIAN_POINT('',(0.288675134594813,0.0590919554682611,-0.5));
#5772=CARTESIAN_POINT('Ctrl Pts',(0.288675134594813,0.0590919554682611,
-0.5));
#5773=CARTESIAN_POINT('Ctrl Pts',(-2.16648921025353E-12,-0.0242413778636962,
-0.5));
#5774=CARTESIAN_POINT('Ctrl Pts',(-0.288675134594813,0.0590919554682611,
-0.5));
#5775=CARTESIAN_POINT('',(0.577350269189626,0.0590919554682611,0.));
#5776=CARTESIAN_POINT('Ctrl Pts',(0.577350269189626,0.0590919554682611,
0.));
#5777=CARTESIAN_POINT('Ctrl Pts',(0.433012701891136,-0.0242413778636963,
-0.250000000001876));
#5778=CARTESIAN_POINT('Ctrl Pts',(0.288675134594813,0.0590919554682611,
-0.5));
#5779=CARTESIAN_POINT('Ctrl Pts',(0.288675134594813,0.0590919554682611,
0.5));
#5780=CARTESIAN_POINT('Ctrl Pts',(0.433012701893303,-0.0242413778636962,
0.249999999998124));
#5781=CARTESIAN_POINT('Ctrl Pts',(0.577350269189626,0.0590919554682611,
0.));
#5782=CARTESIAN_POINT('Origin',(0.,0.461586508806388,0.));
#5783=CARTESIAN_POINT('',(-0.475,0.52,-5.81707229594993E-17));
#5784=CARTESIAN_POINT('Origin',(0.,0.52,0.));
#5785=CARTESIAN_POINT('',(-0.577350269189626,0.460908044531739,-7.07050159149938E-17));
#5786=CARTESIAN_POINT('',(-0.576175134594813,0.461586508806388,-7.05611034329833E-17));
#5787=CARTESIAN_POINT('',(-0.288675134594813,0.460908044531739,0.5));
#5788=CARTESIAN_POINT('Ctrl Pts',(-0.288675134594813,0.460908044531739,
0.5));
#5789=CARTESIAN_POINT('Ctrl Pts',(-0.433012701893303,0.544241377863696,
0.249999999998124));
#5790=CARTESIAN_POINT('Ctrl Pts',(-0.577350269189626,0.460908044531739,
-7.07050159149938E-17));
#5791=CARTESIAN_POINT('',(0.288675134594813,0.460908044531739,0.5));
#5792=CARTESIAN_POINT('Ctrl Pts',(0.288675134594813,0.460908044531739,0.5));
#5793=CARTESIAN_POINT('Ctrl Pts',(-2.16676676600969E-12,0.544241377863697,
0.5));
#5794=CARTESIAN_POINT('Ctrl Pts',(-0.288675134594813,0.460908044531739,
0.5));
#5795=CARTESIAN_POINT('',(0.577350269189626,0.460908044531739,0.));
#5796=CARTESIAN_POINT('Ctrl Pts',(0.577350269189626,0.460908044531739,0.));
#5797=CARTESIAN_POINT('Ctrl Pts',(0.433012701891136,0.544241377863696,0.250000000001876));
#5798=CARTESIAN_POINT('Ctrl Pts',(0.288675134594813,0.460908044531739,0.5));
#5799=CARTESIAN_POINT('',(0.288675134594813,0.460908044531739,-0.5));
#5800=CARTESIAN_POINT('Ctrl Pts',(0.288675134594813,0.460908044531739,-0.5));
#5801=CARTESIAN_POINT('Ctrl Pts',(0.433012701893302,0.544241377863696,-0.249999999998124));
#5802=CARTESIAN_POINT('Ctrl Pts',(0.577350269189626,0.460908044531739,0.));
#5803=CARTESIAN_POINT('',(-0.288675134594813,0.460908044531739,-0.5));
#5804=CARTESIAN_POINT('Ctrl Pts',(-0.288675134594813,0.460908044531739,
-0.5));
#5805=CARTESIAN_POINT('Ctrl Pts',(2.16660023255599E-12,0.544241377863697,
-0.5));
#5806=CARTESIAN_POINT('Ctrl Pts',(0.288675134594813,0.460908044531739,-0.5));
#5807=CARTESIAN_POINT('Ctrl Pts',(-0.577350269189626,0.460908044531739,
-7.07050159149938E-17));
#5808=CARTESIAN_POINT('Ctrl Pts',(-0.433012701891136,0.544241377863696,
-0.250000000001876));
#5809=CARTESIAN_POINT('Ctrl Pts',(-0.288675134594813,0.460908044531739,
-0.5));
#5810=CARTESIAN_POINT('Origin',(0.288675134594813,0.,-0.5));
#5811=CARTESIAN_POINT('',(-0.288675134594813,0.,-0.5));
#5812=CARTESIAN_POINT('',(0.288675134594813,0.,-0.5));
#5813=CARTESIAN_POINT('Origin',(-0.288675134594813,0.,-0.5));
#5814=CARTESIAN_POINT('',(-0.577350269189626,0.,-7.07050159149938E-17));
#5815=CARTESIAN_POINT('Origin',(-0.577350269189626,0.,-7.07050159149938E-17));
#5816=CARTESIAN_POINT('',(-0.288675134594813,0.,0.5));
#5817=CARTESIAN_POINT('Origin',(0.,0.,0.));
#5818=CARTESIAN_POINT('',(-0.25175,0.52,3.08304831685346E-17));
#5819=CARTESIAN_POINT('Origin',(0.,0.52,0.));
#5820=CARTESIAN_POINT('',(-0.25175,0.,3.08304831685346E-17));
#5821=CARTESIAN_POINT('',(-0.25175,0.,3.08304831685346E-17));
#5822=CARTESIAN_POINT('Origin',(0.,0.,0.));
#5823=CARTESIAN_POINT('Origin',(-0.288675134594813,0.,0.5));
#5824=CARTESIAN_POINT('',(0.288675134594813,0.,0.5));
#5825=CARTESIAN_POINT('Origin',(0.577350269189626,0.,0.));
#5826=CARTESIAN_POINT('',(0.577350269189626,0.,0.));
#5827=CARTESIAN_POINT('Origin',(0.288675134594813,0.,0.5));
#5828=CARTESIAN_POINT('Origin',(0.,0.52,0.));
#5829=CARTESIAN_POINT('Origin',(0.,0.,0.));
#5830=CARTESIAN_POINT('',(0.,0.,0.));
#5831=CARTESIAN_POINT('',(0.,0.,0.));
#5832=CARTESIAN_POINT('',(0.,1.72,3.));
#5833=CARTESIAN_POINT('',(0.,1.56,3.));
#5834=CARTESIAN_POINT('',(0.,-1.72,3.));
#5835=CARTESIAN_POINT('',(0.,-2.24,3.));
#5836=CARTESIAN_POINT('',(7.5,0.,0.));
#5837=CARTESIAN_POINT('',(10.,0.,0.));
#5838=CARTESIAN_POINT('',(10.,1.72,3.));
#5839=CARTESIAN_POINT('',(10.,1.56,3.));
#5840=CARTESIAN_POINT('',(10.,-1.72,3.));
#5841=CARTESIAN_POINT('',(10.,-2.24,3.));
#5842=CARTESIAN_POINT('',(10.,0.,0.));
#5843=CARTESIAN_POINT('',(12.5,0.,0.));
#5844=CARTESIAN_POINT('',(12.5,1.72,3.));
#5845=CARTESIAN_POINT('',(12.5,1.56,3.));
#5846=CARTESIAN_POINT('',(12.5,-1.72,3.));
#5847=CARTESIAN_POINT('',(12.5,-2.24,3.));
#5848=CARTESIAN_POINT('',(12.5,0.,0.));
#5849=CARTESIAN_POINT('',(15.,0.,0.));
#5850=CARTESIAN_POINT('',(15.,1.72,3.));
#5851=CARTESIAN_POINT('',(15.,1.56,3.));
#5852=CARTESIAN_POINT('',(15.,-1.72,3.));
#5853=CARTESIAN_POINT('',(15.,-2.24,3.));
#5854=CARTESIAN_POINT('',(15.,0.,0.));
#5855=CARTESIAN_POINT('',(17.5,0.,0.));
#5856=CARTESIAN_POINT('',(17.5,1.72,3.));
#5857=CARTESIAN_POINT('',(17.5,1.56,3.));
#5858=CARTESIAN_POINT('',(17.5,-1.72,3.));
#5859=CARTESIAN_POINT('',(17.5,-2.24,3.));
#5860=CARTESIAN_POINT('',(17.5,0.,0.));
#5861=CARTESIAN_POINT('',(20.,0.,0.));
#5862=CARTESIAN_POINT('',(20.,1.72,3.));
#5863=CARTESIAN_POINT('',(20.,1.56,3.));
#5864=CARTESIAN_POINT('',(20.,-1.72,3.));
#5865=CARTESIAN_POINT('',(20.,-2.24,3.));
#5866=CARTESIAN_POINT('',(0.,0.,0.));
#5867=CARTESIAN_POINT('',(2.5,0.,0.));
#5868=CARTESIAN_POINT('',(2.5,1.72,3.));
#5869=CARTESIAN_POINT('',(2.5,1.56,3.));
#5870=CARTESIAN_POINT('',(2.5,-1.72,3.));
#5871=CARTESIAN_POINT('',(2.5,-2.24,3.));
#5872=CARTESIAN_POINT('',(0.,0.,0.));
#5873=CARTESIAN_POINT('',(0.,0.,0.));
#5874=CARTESIAN_POINT('',(2.34683487000079,7.19069506327294E-15,-0.11439424977191));
#5875=CARTESIAN_POINT('',(-0.249330552480827,1.10906719801976E-14,2.41680664770231));
#5876=CARTESIAN_POINT('',(-1.11314572580792,1.36186369545404E-14,4.00892690157446));
#5877=CARTESIAN_POINT('',(-0.250479636367205,2.00846136561672E-15,2.23634818973092));
#5878=CARTESIAN_POINT('',(-1.87521148215513,6.83212927302934E-15,6.56200215653827));
#5879=CARTESIAN_POINT('',(-2.21825479888781,1.64629740010554E-14,12.6689841621271));
#5880=CARTESIAN_POINT('',(4.16066109449367,-0.160000000000014,1.46366548413505));
#5881=CARTESIAN_POINT('',(6.23109901181892,-0.15999999999998,3.03401679019558));
#5882=UNCERTAINTY_MEASURE_WITH_UNIT(LENGTH_MEASURE(0.001),#5930,
'DISTANCE_ACCURACY_VALUE',
'Maximum model space distance between geometric entities at asserted c
onnectivities');
#5883=UNCERTAINTY_MEASURE_WITH_UNIT(LENGTH_MEASURE(0.001),#5930,
'DISTANCE_ACCURACY_VALUE',
'Maximum model space distance between geometric entities at asserted c
onnectivities');
#5884=UNCERTAINTY_MEASURE_WITH_UNIT(LENGTH_MEASURE(0.001),#5930,
'DISTANCE_ACCURACY_VALUE',
'Maximum model space distance between geometric entities at asserted c
onnectivities');
#5885=UNCERTAINTY_MEASURE_WITH_UNIT(LENGTH_MEASURE(0.001),#5930,
'DISTANCE_ACCURACY_VALUE',
'Maximum model space distance between geometric entities at asserted c
onnectivities');
#5886=UNCERTAINTY_MEASURE_WITH_UNIT(LENGTH_MEASURE(0.001),#5930,
'DISTANCE_ACCURACY_VALUE',
'Maximum model space distance between geometric entities at asserted c
onnectivities');
#5887=UNCERTAINTY_MEASURE_WITH_UNIT(LENGTH_MEASURE(0.001),#5930,
'DISTANCE_ACCURACY_VALUE',
'Maximum model space distance between geometric entities at asserted c
onnectivities');
#5888=UNCERTAINTY_MEASURE_WITH_UNIT(LENGTH_MEASURE(0.001),#5930,
'DISTANCE_ACCURACY_VALUE',
'Maximum model space distance between geometric entities at asserted c
onnectivities');
#5889=UNCERTAINTY_MEASURE_WITH_UNIT(LENGTH_MEASURE(0.001),#5930,
'DISTANCE_ACCURACY_VALUE',
'Maximum model space distance between geometric entities at asserted c
onnectivities');
#5890=UNCERTAINTY_MEASURE_WITH_UNIT(LENGTH_MEASURE(0.001),#5930,
'DISTANCE_ACCURACY_VALUE',
'Maximum model space distance between geometric entities at asserted c
onnectivities');
#5891=UNCERTAINTY_MEASURE_WITH_UNIT(LENGTH_MEASURE(0.001),#5930,
'DISTANCE_ACCURACY_VALUE',
'Maximum model space distance between geometric entities at asserted c
onnectivities');
#5892=UNCERTAINTY_MEASURE_WITH_UNIT(LENGTH_MEASURE(0.001),#5930,
'DISTANCE_ACCURACY_VALUE',
'Maximum model space distance between geometric entities at asserted c
onnectivities');
#5893=UNCERTAINTY_MEASURE_WITH_UNIT(LENGTH_MEASURE(0.001),#5930,
'DISTANCE_ACCURACY_VALUE',
'Maximum model space distance between geometric entities at asserted c
onnectivities');
#5894=UNCERTAINTY_MEASURE_WITH_UNIT(LENGTH_MEASURE(0.001),#5930,
'DISTANCE_ACCURACY_VALUE',
'Maximum model space distance between geometric entities at asserted c
onnectivities');
#5895=UNCERTAINTY_MEASURE_WITH_UNIT(LENGTH_MEASURE(0.001),#5930,
'DISTANCE_ACCURACY_VALUE',
'Maximum model space distance between geometric entities at asserted c
onnectivities');
#5896=UNCERTAINTY_MEASURE_WITH_UNIT(LENGTH_MEASURE(0.001),#5930,
'DISTANCE_ACCURACY_VALUE',
'Maximum model space distance between geometric entities at asserted c
onnectivities');
#5897=UNCERTAINTY_MEASURE_WITH_UNIT(LENGTH_MEASURE(0.001),#5930,
'DISTANCE_ACCURACY_VALUE',
'Maximum model space distance between geometric entities at asserted c
onnectivities');
#5898=UNCERTAINTY_MEASURE_WITH_UNIT(LENGTH_MEASURE(0.001),#5930,
'DISTANCE_ACCURACY_VALUE',
'Maximum model space distance between geometric entities at asserted c
onnectivities');
#5899=UNCERTAINTY_MEASURE_WITH_UNIT(LENGTH_MEASURE(0.001),#5930,
'DISTANCE_ACCURACY_VALUE',
'Maximum model space distance between geometric entities at asserted c
onnectivities');
#5900=UNCERTAINTY_MEASURE_WITH_UNIT(LENGTH_MEASURE(0.001),#5930,
'DISTANCE_ACCURACY_VALUE',
'Maximum model space distance between geometric entities at asserted c
onnectivities');
#5901=UNCERTAINTY_MEASURE_WITH_UNIT(LENGTH_MEASURE(0.001),#5930,
'DISTANCE_ACCURACY_VALUE',
'Maximum model space distance between geometric entities at asserted c
onnectivities');
#5902=UNCERTAINTY_MEASURE_WITH_UNIT(LENGTH_MEASURE(0.001),#5930,
'DISTANCE_ACCURACY_VALUE',
'Maximum model space distance between geometric entities at asserted c
onnectivities');
#5903=UNCERTAINTY_MEASURE_WITH_UNIT(LENGTH_MEASURE(0.001),#5930,
'DISTANCE_ACCURACY_VALUE',
'Maximum model space distance between geometric entities at asserted c
onnectivities');
#5904=UNCERTAINTY_MEASURE_WITH_UNIT(LENGTH_MEASURE(0.001),#5930,
'DISTANCE_ACCURACY_VALUE',
'Maximum model space distance between geometric entities at asserted c
onnectivities');
#5905=UNCERTAINTY_MEASURE_WITH_UNIT(LENGTH_MEASURE(0.001),#5930,
'DISTANCE_ACCURACY_VALUE',
'Maximum model space distance between geometric entities at asserted c
onnectivities');
#5906=(
GEOMETRIC_REPRESENTATION_CONTEXT(3)
GLOBAL_UNCERTAINTY_ASSIGNED_CONTEXT((#5882))
GLOBAL_UNIT_ASSIGNED_CONTEXT((#5930,#5932,#5933))
REPRESENTATION_CONTEXT('','3D')
);
#5907=(
GEOMETRIC_REPRESENTATION_CONTEXT(3)
GLOBAL_UNCERTAINTY_ASSIGNED_CONTEXT((#5883))
GLOBAL_UNIT_ASSIGNED_CONTEXT((#5930,#5932,#5933))
REPRESENTATION_CONTEXT('','3D')
);
#5908=(
GEOMETRIC_REPRESENTATION_CONTEXT(3)
GLOBAL_UNCERTAINTY_ASSIGNED_CONTEXT((#5884))
GLOBAL_UNIT_ASSIGNED_CONTEXT((#5930,#5932,#5933))
REPRESENTATION_CONTEXT('','3D')
);
#5909=(
GEOMETRIC_REPRESENTATION_CONTEXT(3)
GLOBAL_UNCERTAINTY_ASSIGNED_CONTEXT((#5885))
GLOBAL_UNIT_ASSIGNED_CONTEXT((#5930,#5932,#5933))
REPRESENTATION_CONTEXT('','3D')
);
#5910=(
GEOMETRIC_REPRESENTATION_CONTEXT(3)
GLOBAL_UNCERTAINTY_ASSIGNED_CONTEXT((#5886))
GLOBAL_UNIT_ASSIGNED_CONTEXT((#5930,#5932,#5933))
REPRESENTATION_CONTEXT('','3D')
);
#5911=(
GEOMETRIC_REPRESENTATION_CONTEXT(3)
GLOBAL_UNCERTAINTY_ASSIGNED_CONTEXT((#5887))
GLOBAL_UNIT_ASSIGNED_CONTEXT((#5930,#5932,#5933))
REPRESENTATION_CONTEXT('','3D')
);
#5912=(
GEOMETRIC_REPRESENTATION_CONTEXT(3)
GLOBAL_UNCERTAINTY_ASSIGNED_CONTEXT((#5888))
GLOBAL_UNIT_ASSIGNED_CONTEXT((#5930,#5932,#5933))
REPRESENTATION_CONTEXT('','3D')
);
#5913=(
GEOMETRIC_REPRESENTATION_CONTEXT(3)
GLOBAL_UNCERTAINTY_ASSIGNED_CONTEXT((#5889))
GLOBAL_UNIT_ASSIGNED_CONTEXT((#5930,#5932,#5933))
REPRESENTATION_CONTEXT('','3D')
);
#5914=(
GEOMETRIC_REPRESENTATION_CONTEXT(3)
GLOBAL_UNCERTAINTY_ASSIGNED_CONTEXT((#5890))
GLOBAL_UNIT_ASSIGNED_CONTEXT((#5930,#5932,#5933))
REPRESENTATION_CONTEXT('','3D')
);
#5915=(
GEOMETRIC_REPRESENTATION_CONTEXT(3)
GLOBAL_UNCERTAINTY_ASSIGNED_CONTEXT((#5891))
GLOBAL_UNIT_ASSIGNED_CONTEXT((#5930,#5932,#5933))
REPRESENTATION_CONTEXT('','3D')
);
#5916=(
GEOMETRIC_REPRESENTATION_CONTEXT(3)
GLOBAL_UNCERTAINTY_ASSIGNED_CONTEXT((#5892))
GLOBAL_UNIT_ASSIGNED_CONTEXT((#5930,#5932,#5933))
REPRESENTATION_CONTEXT('','3D')
);
#5917=(
GEOMETRIC_REPRESENTATION_CONTEXT(3)
GLOBAL_UNCERTAINTY_ASSIGNED_CONTEXT((#5893))
GLOBAL_UNIT_ASSIGNED_CONTEXT((#5930,#5932,#5933))
REPRESENTATION_CONTEXT('','3D')
);
#5918=(
GEOMETRIC_REPRESENTATION_CONTEXT(3)
GLOBAL_UNCERTAINTY_ASSIGNED_CONTEXT((#5894))
GLOBAL_UNIT_ASSIGNED_CONTEXT((#5930,#5932,#5933))
REPRESENTATION_CONTEXT('','3D')
);
#5919=(
GEOMETRIC_REPRESENTATION_CONTEXT(3)
GLOBAL_UNCERTAINTY_ASSIGNED_CONTEXT((#5895))
GLOBAL_UNIT_ASSIGNED_CONTEXT((#5930,#5932,#5933))
REPRESENTATION_CONTEXT('','3D')
);
#5920=(
GEOMETRIC_REPRESENTATION_CONTEXT(3)
GLOBAL_UNCERTAINTY_ASSIGNED_CONTEXT((#5896))
GLOBAL_UNIT_ASSIGNED_CONTEXT((#5930,#5932,#5933))
REPRESENTATION_CONTEXT('','3D')
);
#5921=(
GEOMETRIC_REPRESENTATION_CONTEXT(3)
GLOBAL_UNCERTAINTY_ASSIGNED_CONTEXT((#5897))
GLOBAL_UNIT_ASSIGNED_CONTEXT((#5930,#5932,#5933))
REPRESENTATION_CONTEXT('','3D')
);
#5922=(
GEOMETRIC_REPRESENTATION_CONTEXT(3)
GLOBAL_UNCERTAINTY_ASSIGNED_CONTEXT((#5898))
GLOBAL_UNIT_ASSIGNED_CONTEXT((#5930,#5932,#5933))
REPRESENTATION_CONTEXT('','3D')
);
#5923=(
GEOMETRIC_REPRESENTATION_CONTEXT(3)
GLOBAL_UNCERTAINTY_ASSIGNED_CONTEXT((#5899))
GLOBAL_UNIT_ASSIGNED_CONTEXT((#5930,#5932,#5933))
REPRESENTATION_CONTEXT('','3D')
);
#5924=(
GEOMETRIC_REPRESENTATION_CONTEXT(3)
GLOBAL_UNCERTAINTY_ASSIGNED_CONTEXT((#5900))
GLOBAL_UNIT_ASSIGNED_CONTEXT((#5930,#5932,#5933))
REPRESENTATION_CONTEXT('','3D')
);
#5925=(
GEOMETRIC_REPRESENTATION_CONTEXT(3)
GLOBAL_UNCERTAINTY_ASSIGNED_CONTEXT((#5901))
GLOBAL_UNIT_ASSIGNED_CONTEXT((#5930,#5932,#5933))
REPRESENTATION_CONTEXT('','3D')
);
#5926=(
GEOMETRIC_REPRESENTATION_CONTEXT(3)
GLOBAL_UNCERTAINTY_ASSIGNED_CONTEXT((#5902))
GLOBAL_UNIT_ASSIGNED_CONTEXT((#5930,#5932,#5933))
REPRESENTATION_CONTEXT('','3D')
);
#5927=(
GEOMETRIC_REPRESENTATION_CONTEXT(3)
GLOBAL_UNCERTAINTY_ASSIGNED_CONTEXT((#5903))
GLOBAL_UNIT_ASSIGNED_CONTEXT((#5930,#5932,#5933))
REPRESENTATION_CONTEXT('','3D')
);
#5928=(
GEOMETRIC_REPRESENTATION_CONTEXT(3)
GLOBAL_UNCERTAINTY_ASSIGNED_CONTEXT((#5904))
GLOBAL_UNIT_ASSIGNED_CONTEXT((#5930,#5932,#5933))
REPRESENTATION_CONTEXT('','3D')
);
#5929=(
GEOMETRIC_REPRESENTATION_CONTEXT(3)
GLOBAL_UNCERTAINTY_ASSIGNED_CONTEXT((#5905))
GLOBAL_UNIT_ASSIGNED_CONTEXT((#5930,#5932,#5933))
REPRESENTATION_CONTEXT('','3D')
);
#5930=(
LENGTH_UNIT()
NAMED_UNIT(*)
SI_UNIT(.CENTI.,.METRE.)
);
#5931=(
LENGTH_UNIT()
NAMED_UNIT(*)
SI_UNIT($,.METRE.)
);
#5932=(
NAMED_UNIT(*)
PLANE_ANGLE_UNIT()
SI_UNIT($,.RADIAN.)
);
#5933=(
NAMED_UNIT(*)
SI_UNIT($,.STERADIAN.)
SOLID_ANGLE_UNIT()
);
#5934=SHAPE_DEFINITION_REPRESENTATION(#5957,#6039);
#5935=SHAPE_DEFINITION_REPRESENTATION(#5958,#6040);
#5936=SHAPE_DEFINITION_REPRESENTATION(#5959,#6041);
#5937=SHAPE_DEFINITION_REPRESENTATION(#5960,#6042);
#5938=SHAPE_DEFINITION_REPRESENTATION(#5961,#6043);
#5939=SHAPE_DEFINITION_REPRESENTATION(#5962,#6044);
#5940=SHAPE_DEFINITION_REPRESENTATION(#5963,#6045);
#5941=SHAPE_DEFINITION_REPRESENTATION(#5964,#6046);
#5942=SHAPE_DEFINITION_REPRESENTATION(#5965,#6047);
#5943=SHAPE_DEFINITION_REPRESENTATION(#5966,#6048);
#5944=SHAPE_DEFINITION_REPRESENTATION(#5973,#6049);
#5945=SHAPE_DEFINITION_REPRESENTATION(#5974,#6050);
#5946=SHAPE_DEFINITION_REPRESENTATION(#5975,#6051);
#5947=SHAPE_DEFINITION_REPRESENTATION(#5976,#6052);
#5948=SHAPE_DEFINITION_REPRESENTATION(#5977,#6053);
#5949=SHAPE_DEFINITION_REPRESENTATION(#5978,#6054);
#5950=SHAPE_DEFINITION_REPRESENTATION(#5979,#6055);
#5951=SHAPE_DEFINITION_REPRESENTATION(#5981,#6056);
#5952=SHAPE_DEFINITION_REPRESENTATION(#5982,#6057);
#5953=SHAPE_DEFINITION_REPRESENTATION(#5983,#6058);
#5954=SHAPE_DEFINITION_REPRESENTATION(#5984,#6059);
#5955=SHAPE_DEFINITION_REPRESENTATION(#5985,#6060);
#5956=SHAPE_DEFINITION_REPRESENTATION(#5986,#6061);
#5957=PRODUCT_DEFINITION_SHAPE('',$,#6063);
#5958=PRODUCT_DEFINITION_SHAPE('',$,#6064);
#5959=PRODUCT_DEFINITION_SHAPE('',$,#6065);
#5960=PRODUCT_DEFINITION_SHAPE('',$,#6066);
#5961=PRODUCT_DEFINITION_SHAPE('',$,#6067);
#5962=PRODUCT_DEFINITION_SHAPE('',$,#6068);
#5963=PRODUCT_DEFINITION_SHAPE('',$,#6069);
#5964=PRODUCT_DEFINITION_SHAPE('',$,#6070);
#5965=PRODUCT_DEFINITION_SHAPE('',$,#6071);
#5966=PRODUCT_DEFINITION_SHAPE('',$,#6072);
#5967=PRODUCT_DEFINITION_SHAPE($,$,#188);
#5968=PRODUCT_DEFINITION_SHAPE($,$,#189);
#5969=PRODUCT_DEFINITION_SHAPE($,$,#190);
#5970=PRODUCT_DEFINITION_SHAPE($,$,#191);
#5971=PRODUCT_DEFINITION_SHAPE($,$,#192);
#5972=PRODUCT_DEFINITION_SHAPE($,$,#193);
#5973=PRODUCT_DEFINITION_SHAPE('',$,#6073);
#5974=PRODUCT_DEFINITION_SHAPE('',$,#6074);
#5975=PRODUCT_DEFINITION_SHAPE('',$,#6075);
#5976=PRODUCT_DEFINITION_SHAPE('',$,#6076);
#5977=PRODUCT_DEFINITION_SHAPE('',$,#6077);
#5978=PRODUCT_DEFINITION_SHAPE('',$,#6078);
#5979=PRODUCT_DEFINITION_SHAPE('',$,#6079);
#5980=PRODUCT_DEFINITION_SHAPE($,$,#194);
#5981=PRODUCT_DEFINITION_SHAPE('',$,#6080);
#5982=PRODUCT_DEFINITION_SHAPE('',$,#6081);
#5983=PRODUCT_DEFINITION_SHAPE('',$,#6082);
#5984=PRODUCT_DEFINITION_SHAPE('',$,#6083);
#5985=PRODUCT_DEFINITION_SHAPE('',$,#6084);
#5986=PRODUCT_DEFINITION_SHAPE('',$,#6085);
#5987=PRODUCT_DEFINITION_SHAPE($,$,#195);
#5988=PRODUCT_DEFINITION_SHAPE($,$,#196);
#5989=PRODUCT_DEFINITION_SHAPE($,$,#197);
#5990=PRODUCT_DEFINITION_SHAPE($,$,#198);
#5991=PRODUCT_DEFINITION_SHAPE($,$,#199);
#5992=PRODUCT_DEFINITION_SHAPE($,$,#200);
#5993=PRODUCT_DEFINITION_SHAPE($,$,#201);
#5994=PRODUCT_DEFINITION_SHAPE($,$,#202);
#5995=PRODUCT_DEFINITION_SHAPE($,$,#203);
#5996=PRODUCT_DEFINITION_SHAPE($,$,#204);
#5997=PRODUCT_DEFINITION_SHAPE($,$,#205);
#5998=PRODUCT_DEFINITION_SHAPE($,$,#206);
#5999=PRODUCT_DEFINITION_SHAPE($,$,#207);
#6000=PRODUCT_DEFINITION_SHAPE($,$,#208);
#6001=PRODUCT_DEFINITION_SHAPE($,$,#209);
#6002=PRODUCT_DEFINITION_SHAPE($,$,#210);
#6003=PRODUCT_DEFINITION_SHAPE($,$,#211);
#6004=PRODUCT_DEFINITION_SHAPE($,$,#212);
#6005=PRODUCT_DEFINITION_SHAPE($,$,#213);
#6006=PRODUCT_DEFINITION_SHAPE($,$,#214);
#6007=PRODUCT_DEFINITION_SHAPE($,$,#215);
#6008=PRODUCT_DEFINITION_SHAPE($,$,#216);
#6009=PRODUCT_DEFINITION_SHAPE($,$,#217);
#6010=PRODUCT_DEFINITION_SHAPE($,$,#218);
#6011=PRODUCT_DEFINITION_SHAPE($,$,#219);
#6012=PRODUCT_DEFINITION_SHAPE($,$,#220);
#6013=PRODUCT_DEFINITION_SHAPE($,$,#221);
#6014=PRODUCT_DEFINITION_SHAPE($,$,#222);
#6015=PRODUCT_DEFINITION_SHAPE($,$,#223);
#6016=PRODUCT_DEFINITION_SHAPE($,$,#224);
#6017=PRODUCT_DEFINITION_SHAPE($,$,#225);
#6018=PRODUCT_DEFINITION_SHAPE($,$,#226);
#6019=PRODUCT_DEFINITION_SHAPE($,$,#227);
#6020=PRODUCT_DEFINITION_SHAPE($,$,#228);
#6021=PRODUCT_DEFINITION_SHAPE($,$,#229);
#6022=PRODUCT_DEFINITION_SHAPE($,$,#230);
#6023=PRODUCT_DEFINITION_SHAPE($,$,#231);
#6024=PRODUCT_DEFINITION_SHAPE($,$,#232);
#6025=PRODUCT_DEFINITION_SHAPE($,$,#233);
#6026=PRODUCT_DEFINITION_SHAPE($,$,#234);
#6027=PRODUCT_DEFINITION_SHAPE($,$,#235);
#6028=PRODUCT_DEFINITION_SHAPE($,$,#236);
#6029=PRODUCT_DEFINITION_SHAPE($,$,#237);
#6030=PRODUCT_DEFINITION_SHAPE($,$,#238);
#6031=PRODUCT_DEFINITION_SHAPE($,$,#239);
#6032=PRODUCT_DEFINITION_SHAPE($,$,#240);
#6033=PRODUCT_DEFINITION_SHAPE($,$,#241);
#6034=PRODUCT_DEFINITION_SHAPE($,$,#242);
#6035=PRODUCT_DEFINITION_SHAPE($,$,#243);
#6036=PRODUCT_DEFINITION_SHAPE($,$,#244);
#6037=PRODUCT_DEFINITION_SHAPE($,$,#245);
#6038=PRODUCT_DEFINITION_SHAPE($,$,#246);
#6039=SHAPE_REPRESENTATION('',(#3422,#3804,#3805,#3806,#3807,#3808,#3809,
#3810,#3811,#3812,#3813),#5906);
#6040=SHAPE_REPRESENTATION('',(#3423,#3762,#3763,#3764,#3765,#3766,#3767),
#5907);
#6041=SHAPE_REPRESENTATION('',(#3424),#5908);
#6042=SHAPE_REPRESENTATION('',(#3459,#3591,#3592,#3593,#3594,#3595,#3596),
#5909);
#6043=SHAPE_REPRESENTATION('',(#3460),#5910);
#6044=SHAPE_REPRESENTATION('',(#3527),#5911);
#6045=SHAPE_REPRESENTATION('',(#3536),#5912);
#6046=SHAPE_REPRESENTATION('',(#3557),#5913);
#6047=SHAPE_REPRESENTATION('',(#3566),#5914);
#6048=SHAPE_REPRESENTATION('',(#3575),#5915);
#6049=SHAPE_REPRESENTATION('',(#3597,#3768,#3769,#3770,#3771,#3772,#3773),
#5916);
#6050=SHAPE_REPRESENTATION('',(#3598,#3774,#3775,#3776,#3777,#3778,#3779),
#5917);
#6051=SHAPE_REPRESENTATION('',(#3599,#3780,#3781,#3782,#3783,#3784,#3785),
#5918);
#6052=SHAPE_REPRESENTATION('',(#3600,#3786,#3787,#3788,#3789,#3790,#3791),
#5919);
#6053=SHAPE_REPRESENTATION('',(#3601,#3792,#3793,#3794,#3795,#3796,#3797),
#5920);
#6054=SHAPE_REPRESENTATION('',(#3602,#3638),#5921);
#6055=SHAPE_REPRESENTATION('',(#3603),#5922);
#6056=SHAPE_REPRESENTATION('',(#3639,#3798,#3799,#3800,#3801,#3802,#3803),
#5923);
#6057=SHAPE_REPRESENTATION('',(#3640),#5924);
#6058=SHAPE_REPRESENTATION('',(#3707),#5925);
#6059=SHAPE_REPRESENTATION('',(#3716),#5926);
#6060=SHAPE_REPRESENTATION('',(#3737),#5927);
#6061=SHAPE_REPRESENTATION('',(#3746),#5928);
#6062=PRODUCT_DEFINITION_CONTEXT('part definition',#6133,'design');
#6063=PRODUCT_DEFINITION('PAT-020',
'PAT-020',#6086,#6062);
#6064=PRODUCT_DEFINITION('Fixed chain bracket','Fixed chain bracket',#6087,
#6062);
#6065=PRODUCT_DEFINITION('Fixed end bracket','Fixed end bracket',#6088,
#6062);
#6066=PRODUCT_DEFINITION('Cable link 1','Cable link 1',#6089,#6062);
#6067=PRODUCT_DEFINITION('Offset cable chain link',
'Offset cable chain link',#6090,#6062);
#6068=PRODUCT_DEFINITION('Hinge bearing sleeve','Hinge bearing sleeve',
#6091,#6062);
#6069=PRODUCT_DEFINITION('Forty millimetre hinge bolt',
'Forty millimetre hinge bolt',#6092,#6062);
#6070=PRODUCT_DEFINITION('Flat Washer - M6','Flat Washer - M6',#6093,#6062);
#6071=PRODUCT_DEFINITION('Flat Washer - M6','Flat Washer - M6',#6094,
#6062);
#6072=PRODUCT_DEFINITION('Hex Nut - M6','Hex Nut - M6',#6095,#6062);
#6073=PRODUCT_DEFINITION('Cable link 4','Cable link 4',#6096,#6062);
#6074=PRODUCT_DEFINITION('Cable link 5','Cable link 5',#6097,#6062);
#6075=PRODUCT_DEFINITION('Cable link 6','Cable link 6',#6098,#6062);
#6076=PRODUCT_DEFINITION('Cable link 7','Cable link 7',#6099,#6062);
#6077=PRODUCT_DEFINITION('Cable link 8','Cable link 8',#6100,#6062);
#6078=PRODUCT_DEFINITION('Moving chain bracket','Moving chain bracket',
#6101,#6062);
#6079=PRODUCT_DEFINITION('Moving end bracket','Moving end bracket',#6102,
#6062);
#6080=PRODUCT_DEFINITION('Cable link 1','Cable link 1',#6103,#6062);
#6081=PRODUCT_DEFINITION('Offset cable chain link',
'Offset cable chain link',#6104,#6062);
#6082=PRODUCT_DEFINITION('Hinge bearing sleeve',
'Hinge bearing sleeve',#6105,#6062);
#6083=PRODUCT_DEFINITION('Forty millimetre hinge bolt',
'Forty millimetre hinge bolt',#6106,#6062);
#6084=PRODUCT_DEFINITION('Flat Washer - M6','Flat Washer - M6',#6107,
#6062);
#6085=PRODUCT_DEFINITION('Hex Nut - M6','Hex Nut - M6',#6108,#6062);
#6086=PRODUCT_DEFINITION_FORMATION('',$,#6135);
#6087=PRODUCT_DEFINITION_FORMATION('',$,#6136);
#6088=PRODUCT_DEFINITION_FORMATION('',$,#6137);
#6089=PRODUCT_DEFINITION_FORMATION('',$,#6138);
#6090=PRODUCT_DEFINITION_FORMATION('',$,#6139);
#6091=PRODUCT_DEFINITION_FORMATION('',$,#6140);
#6092=PRODUCT_DEFINITION_FORMATION('',$,#6141);
#6093=PRODUCT_DEFINITION_FORMATION('',$,#6142);
#6094=PRODUCT_DEFINITION_FORMATION('',$,#6143);
#6095=PRODUCT_DEFINITION_FORMATION('',$,#6144);
#6096=PRODUCT_DEFINITION_FORMATION('',$,#6145);
#6097=PRODUCT_DEFINITION_FORMATION('',$,#6146);
#6098=PRODUCT_DEFINITION_FORMATION('',$,#6147);
#6099=PRODUCT_DEFINITION_FORMATION('',$,#6148);
#6100=PRODUCT_DEFINITION_FORMATION('',$,#6149);
#6101=PRODUCT_DEFINITION_FORMATION('',$,#6150);
#6102=PRODUCT_DEFINITION_FORMATION('',$,#6151);
#6103=PRODUCT_DEFINITION_FORMATION('',$,#6152);
#6104=PRODUCT_DEFINITION_FORMATION('',$,#6153);
#6105=PRODUCT_DEFINITION_FORMATION('',$,#6154);
#6106=PRODUCT_DEFINITION_FORMATION('',$,#6155);
#6107=PRODUCT_DEFINITION_FORMATION('',$,#6156);
#6108=PRODUCT_DEFINITION_FORMATION('',$,#6157);
#6109=PRODUCT_RELATED_PRODUCT_CATEGORY('PAT-020',
'PAT-020',(#6135));
#6110=PRODUCT_RELATED_PRODUCT_CATEGORY('Fixed chain bracket',
'Fixed chain bracket',(#6136));
#6111=PRODUCT_RELATED_PRODUCT_CATEGORY('Fixed end bracket',
'Fixed end bracket',(#6137));
#6112=PRODUCT_RELATED_PRODUCT_CATEGORY('Cable link 1','Cable link 1',(#6138));
#6113=PRODUCT_RELATED_PRODUCT_CATEGORY('Offset cable chain link',
'Offset cable chain link',(#6139));
#6114=PRODUCT_RELATED_PRODUCT_CATEGORY('Hinge bearing sleeve',
'Hinge bearing sleeve',(#6140));
#6115=PRODUCT_RELATED_PRODUCT_CATEGORY('Forty millimetre hinge bolt',
'Forty millimetre hinge bolt',(#6141));
#6116=PRODUCT_RELATED_PRODUCT_CATEGORY('Flat Washer - M6',
'Flat Washer - M6',(#6142));
#6117=PRODUCT_RELATED_PRODUCT_CATEGORY('Flat Washer - M6',
'Flat Washer - M6',(#6143));
#6118=PRODUCT_RELATED_PRODUCT_CATEGORY('Hex Nut - M6','Hex Nut - M6',(#6144));
#6119=PRODUCT_RELATED_PRODUCT_CATEGORY('Cable link 4','Cable link 4',(#6145));
#6120=PRODUCT_RELATED_PRODUCT_CATEGORY('Cable link 5','Cable link 5',(#6146));
#6121=PRODUCT_RELATED_PRODUCT_CATEGORY('Cable link 6','Cable link 6',(#6147));
#6122=PRODUCT_RELATED_PRODUCT_CATEGORY('Cable link 7','Cable link 7',(#6148));
#6123=PRODUCT_RELATED_PRODUCT_CATEGORY('Cable link 8','Cable link 8',(#6149));
#6124=PRODUCT_RELATED_PRODUCT_CATEGORY('Moving chain bracket',
'Moving chain bracket',(#6150));
#6125=PRODUCT_RELATED_PRODUCT_CATEGORY('Moving end bracket',
'Moving end bracket',(#6151));
#6126=PRODUCT_RELATED_PRODUCT_CATEGORY('Cable link 1','Cable link 1',(#6152));
#6127=PRODUCT_RELATED_PRODUCT_CATEGORY('Offset cable chain link',
'Offset cable chain link',(#6153));
#6128=PRODUCT_RELATED_PRODUCT_CATEGORY('Hinge bearing sleeve',
'Hinge bearing sleeve',(#6154));
#6129=PRODUCT_RELATED_PRODUCT_CATEGORY('Forty millimetre hinge bolt',
'Forty millimetre hinge bolt',(#6155));
#6130=PRODUCT_RELATED_PRODUCT_CATEGORY('Flat Washer - M6',
'Flat Washer - M6',(#6156));
#6131=PRODUCT_RELATED_PRODUCT_CATEGORY('Hex Nut - M6','Hex Nut - M6',(#6157));
#6132=APPLICATION_PROTOCOL_DEFINITION('international standard',
'automotive_design',2009,#6133);
#6133=APPLICATION_CONTEXT(
'Core Data for Automotive Mechanical Design Process');
#6134=PRODUCT_CONTEXT('part definition',#6133,'mechanical');
#6135=PRODUCT('PAT-020','PAT-020',
'PAT-020',(#6134));
#6136=PRODUCT('Fixed chain bracket','Fixed chain bracket',
'Fixed chain bracket',(#6134));
#6137=PRODUCT('Fixed end bracket','Fixed end bracket',
'Fixed end bracket',(#6134));
#6138=PRODUCT('Cable link 1','Cable link 1','Cable link 1',(#6134));
#6139=PRODUCT('Offset cable chain link','Offset cable chain link',
'Offset cable chain link',(#6134));
#6140=PRODUCT('Hinge bearing sleeve','Hinge bearing sleeve',
'Hinge bearing sleeve',(#6134));
#6141=PRODUCT('Forty millimetre hinge bolt',
'Forty millimetre hinge bolt','Forty millimetre hinge bolt',(#6134));
#6142=PRODUCT('Flat Washer - M6','Flat Washer - M6','Flat Washer - M6',
(#6134));
#6143=PRODUCT('Flat Washer - M6','Flat Washer - M6',
'Flat Washer - M6',(#6134));
#6144=PRODUCT('Hex Nut - M6','Hex Nut - M6','Hex Nut - M6',(#6134));
#6145=PRODUCT('Cable link 4','Cable link 4','Cable link 4',(#6134));
#6146=PRODUCT('Cable link 5','Cable link 5','Cable link 5',(#6134));
#6147=PRODUCT('Cable link 6','Cable link 6','Cable link 6',(#6134));
#6148=PRODUCT('Cable link 7','Cable link 7','Cable link 7',(#6134));
#6149=PRODUCT('Cable link 8','Cable link 8','Cable link 8',(#6134));
#6150=PRODUCT('Moving chain bracket','Moving chain bracket',
'Moving chain bracket',(#6134));
#6151=PRODUCT('Moving end bracket','Moving end bracket',
'Moving end bracket',(#6134));
#6152=PRODUCT('Cable link 1','Cable link 1','Cable link 1',(#6134));
#6153=PRODUCT('Offset cable chain link','Offset cable chain link',
'Offset cable chain link',(#6134));
#6154=PRODUCT('Hinge bearing sleeve','Hinge bearing sleeve',
'Hinge bearing sleeve',(#6134));
#6155=PRODUCT('Forty millimetre hinge bolt',
'Forty millimetre hinge bolt','Forty millimetre hinge bolt',(#6134));
#6156=PRODUCT('Flat Washer - M6','Flat Washer - M6',
'Flat Washer - M6',(#6134));
#6157=PRODUCT('Hex Nut - M6','Hex Nut - M6','Hex Nut - M6',(#6134));
#6158=PRESENTATION_STYLE_ASSIGNMENT((#6163));
#6159=PRESENTATION_STYLE_ASSIGNMENT((#6164));
#6160=PRESENTATION_STYLE_ASSIGNMENT((#6165));
#6161=PRESENTATION_STYLE_ASSIGNMENT((#6166));
#6162=PRESENTATION_STYLE_ASSIGNMENT((#6167));
#6163=SURFACE_STYLE_USAGE(.BOTH.,#6168);
#6164=SURFACE_STYLE_USAGE(.BOTH.,#6169);
#6165=SURFACE_STYLE_USAGE(.BOTH.,#6170);
#6166=SURFACE_STYLE_USAGE(.BOTH.,#6171);
#6167=SURFACE_STYLE_USAGE(.BOTH.,#6172);
#6168=SURFACE_SIDE_STYLE('',(#6173));
#6169=SURFACE_SIDE_STYLE('',(#6174));
#6170=SURFACE_SIDE_STYLE('',(#6175));
#6171=SURFACE_SIDE_STYLE('',(#6176));
#6172=SURFACE_SIDE_STYLE('',(#6177));
#6173=SURFACE_STYLE_FILL_AREA(#6178);
#6174=SURFACE_STYLE_FILL_AREA(#6179);
#6175=SURFACE_STYLE_FILL_AREA(#6180);
#6176=SURFACE_STYLE_FILL_AREA(#6181);
#6177=SURFACE_STYLE_FILL_AREA(#6182);
#6178=FILL_AREA_STYLE('Steel - Satin',(#6183));
#6179=FILL_AREA_STYLE('CAD Library Painted - Engineering blue',(#6184));
#6180=FILL_AREA_STYLE('CAD Library Painted - Steel gray',(#6185));
#6181=FILL_AREA_STYLE('CAD Library Painted - Graphite',(#6186));
#6182=FILL_AREA_STYLE('CAD Library Painted - Light blue',(#6187));
#6183=FILL_AREA_STYLE_COLOUR('Steel - Satin',#6188);
#6184=FILL_AREA_STYLE_COLOUR('CAD Library Painted - Engineering blue',#6189);
#6185=FILL_AREA_STYLE_COLOUR('CAD Library Painted - Steel gray',#6190);
#6186=FILL_AREA_STYLE_COLOUR('CAD Library Painted - Graphite',#6191);
#6187=FILL_AREA_STYLE_COLOUR('CAD Library Painted - Light blue',#6192);
#6188=COLOUR_RGB('Steel - Satin',0.627450980392157,0.627450980392157,0.627450980392157);
#6189=COLOUR_RGB('CAD Library Painted - Engineering blue',0.12156862745098,
0.356862745098039,0.6);
#6190=COLOUR_RGB('CAD Library Painted - Steel gray',0.592156862745098,0.631372549019608,
0.67843137254902);
#6191=COLOUR_RGB('CAD Library Painted - Graphite',0.0980392156862745,0.109803921568627,
0.125490196078431);
#6192=COLOUR_RGB('CAD Library Painted - Light blue',0.286274509803922,0.552941176470588,
0.780392156862745);
#6193=COLOUR_RGB('Dark Blue',0.08,0.2,0.34);
#6194=FILL_AREA_STYLE_COLOUR('',#6193);
#6195=FILL_AREA_STYLE('',(#6194));
#6196=SURFACE_STYLE_FILL_AREA(#6195);
#6197=SURFACE_SIDE_STYLE('',(#6196));
#6198=SURFACE_STYLE_USAGE(.BOTH.,#6197);
#6199=PRESENTATION_STYLE_ASSIGNMENT((#6198));
#6200=COLOUR_RGB('Light Blue',0.38,0.62,0.78);
#6201=FILL_AREA_STYLE_COLOUR('',#6200);
#6202=FILL_AREA_STYLE('',(#6201));
#6203=SURFACE_STYLE_FILL_AREA(#6202);
#6204=SURFACE_SIDE_STYLE('',(#6203));
#6205=SURFACE_STYLE_USAGE(.BOTH.,#6204);
#6206=PRESENTATION_STYLE_ASSIGNMENT((#6205));
#6207=COLOUR_RGB('Sky Blue',0.24,0.69,0.87);
#6208=FILL_AREA_STYLE_COLOUR('',#6207);
#6209=FILL_AREA_STYLE('',(#6208));
#6210=SURFACE_STYLE_FILL_AREA(#6209);
#6211=SURFACE_SIDE_STYLE('',(#6210));
#6212=SURFACE_STYLE_USAGE(.BOTH.,#6211);
#6213=PRESENTATION_STYLE_ASSIGNMENT((#6212));
#6214=COLOUR_RGB('Grey',0.48,0.52,0.57);
#6215=FILL_AREA_STYLE_COLOUR('',#6214);
#6216=FILL_AREA_STYLE('',(#6215));
#6217=SURFACE_STYLE_FILL_AREA(#6216);
#6218=SURFACE_SIDE_STYLE('',(#6217));
#6219=SURFACE_STYLE_USAGE(.BOTH.,#6218);
#6220=PRESENTATION_STYLE_ASSIGNMENT((#6219));
#6221=COLOUR_RGB('Black',0.12,0.14,0.17);
#6222=FILL_AREA_STYLE_COLOUR('',#6221);
#6223=FILL_AREA_STYLE('',(#6222));
#6224=SURFACE_STYLE_FILL_AREA(#6223);
#6225=SURFACE_SIDE_STYLE('',(#6224));
#6226=SURFACE_STYLE_USAGE(.BOTH.,#6225);
#6227=PRESENTATION_STYLE_ASSIGNMENT((#6226));
#6228=COLOUR_RGB('Off White',0.89,0.88,0.83);
#6229=FILL_AREA_STYLE_COLOUR('',#6228);
#6230=FILL_AREA_STYLE('',(#6229));
#6231=SURFACE_STYLE_FILL_AREA(#6230);
#6232=SURFACE_SIDE_STYLE('',(#6231));
#6233=SURFACE_STYLE_USAGE(.BOTH.,#6232);
#6234=PRESENTATION_STYLE_ASSIGNMENT((#6233));
ENDSEC;
END-ISO-10303-21;
